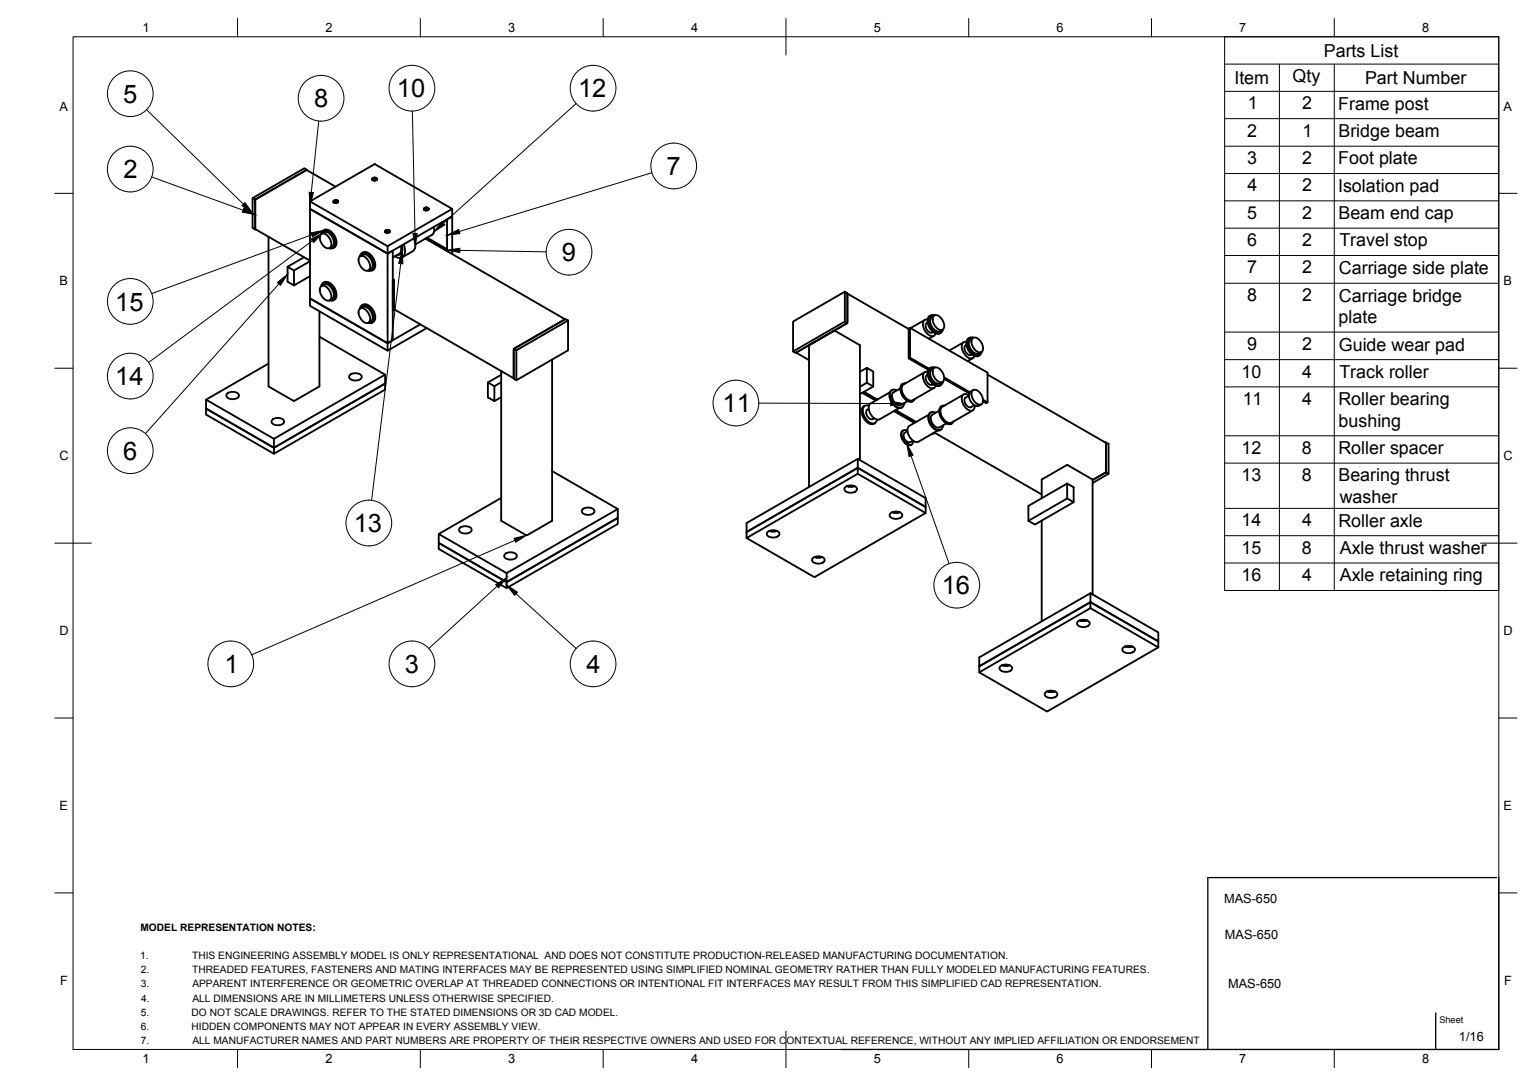
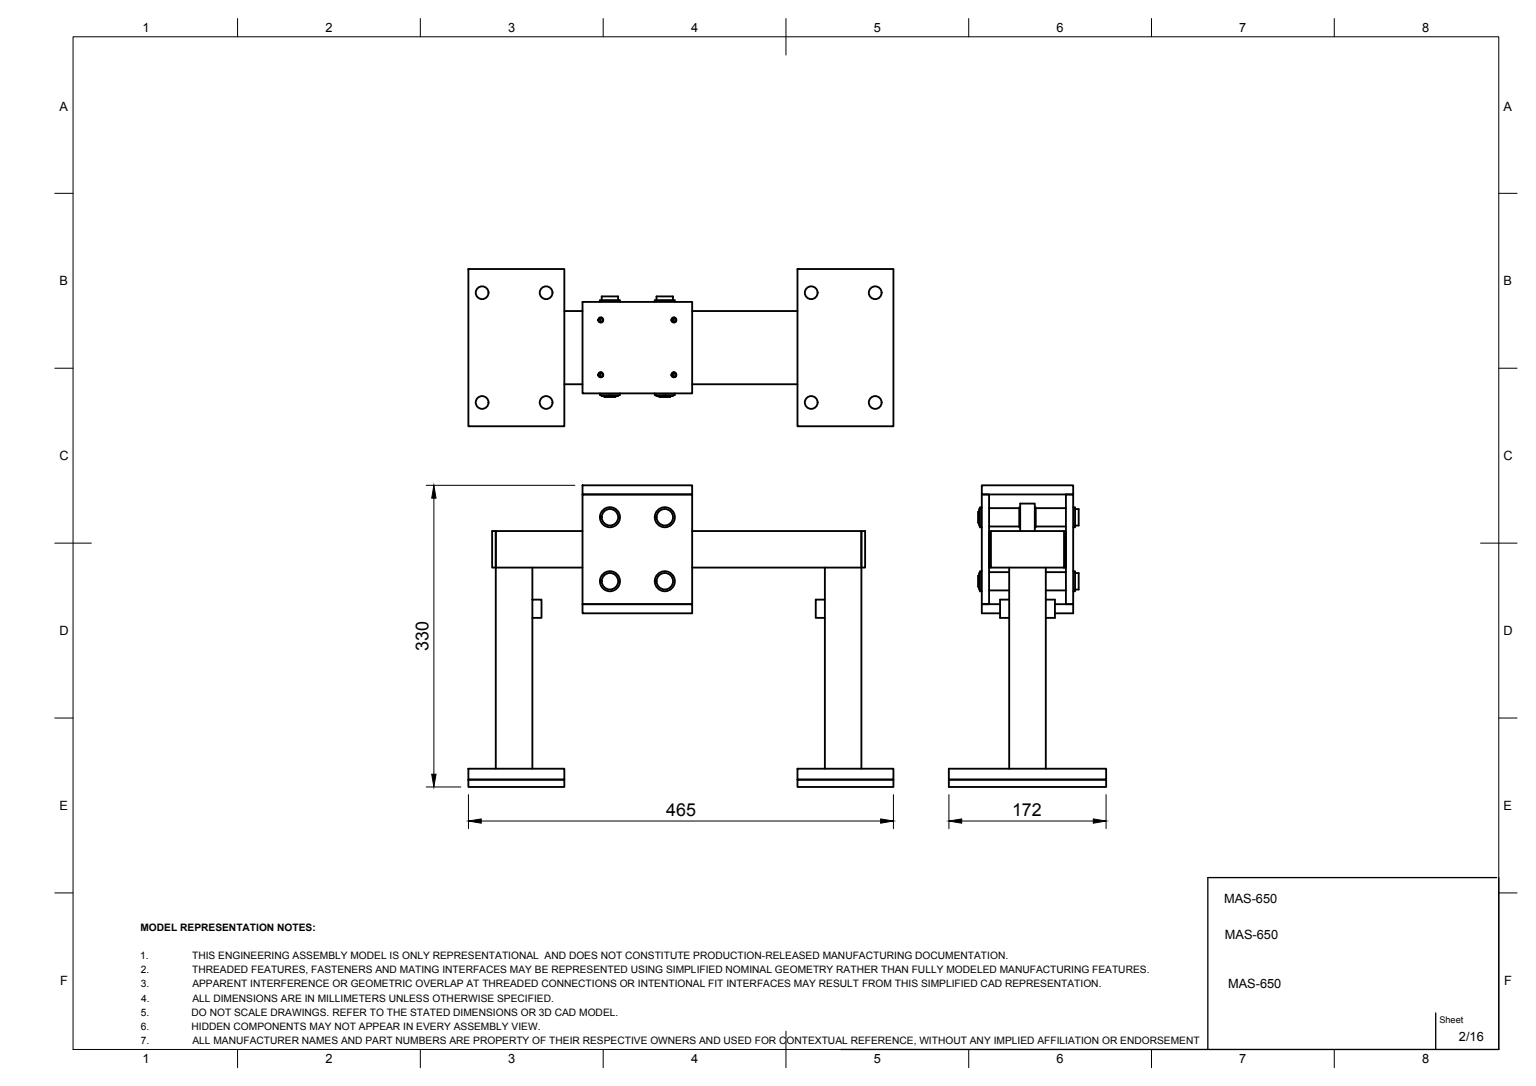
ISO-10303-21;
HEADER;
/* Generated by software containing ST-Developer
 * from STEP Tools, Inc. (www.steptools.com) 
 */

FILE_DESCRIPTION(
/* description */ ('Independent manual traversing gantry with native reusable aluminum pr
ofiles,180mm captured carriage travel, four bronze-bushed rollers, lin
ked ideal rolling motion, bonded acetal lateral guides, positive welde
d end stops and fully retained axle stacks. Editable native profile cu
t lengths220/400mm. Tool attachments viaM6 bridge-plate taps; mounted 
tool outside assembly. Welds, anchors, adhesives, fits, traction, load
/speed/structural/life ratings unassigned.'),
/* implementation_level */ '2;1');

FILE_NAME(
/* name */ 'MAS-650.step',
/* time_stamp */ '2026-11-09T20:04:38-08:00',
/* author */ (''),
/* organization */ (''),
/* preprocessor_version */ 'ST-DEVELOPER v20.2',
/* originating_system */ 'Autodesk Translation Framework v15.17.0.0',
/* authorisation */ '');

FILE_SCHEMA (('AUTOMOTIVE_DESIGN { 1 0 10303 214 3 1 1 }'));
ENDSEC;

DATA;
#10=MECHANICAL_DESIGN_GEOMETRIC_PRESENTATION_REPRESENTATION('',(#471,#472,
#473,#474,#475,#476,#477,#478,#479,#480,#481,#482,#483,#484,#485,#486),
#13231);
#11=ITEM_DEFINED_TRANSFORMATION($,$,#4380,#4678);
#12=ITEM_DEFINED_TRANSFORMATION($,$,#4345,#4679);
#13=ITEM_DEFINED_TRANSFORMATION($,$,#4380,#4680);
#14=ITEM_DEFINED_TRANSFORMATION($,$,#4415,#4681);
#15=ITEM_DEFINED_TRANSFORMATION($,$,#4434,#4682);
#16=ITEM_DEFINED_TRANSFORMATION($,$,#4453,#4683);
#17=ITEM_DEFINED_TRANSFORMATION($,$,#4460,#4684);
#18=ITEM_DEFINED_TRANSFORMATION($,$,#4467,#4685);
#19=ITEM_DEFINED_TRANSFORMATION($,$,#4486,#4686);
#20=ITEM_DEFINED_TRANSFORMATION($,$,#4597,#4687);
#21=ITEM_DEFINED_TRANSFORMATION($,$,#4604,#4688);
#22=ITEM_DEFINED_TRANSFORMATION($,$,#4613,#4689);
#23=ITEM_DEFINED_TRANSFORMATION($,$,#4651,#4690);
#24=ITEM_DEFINED_TRANSFORMATION($,$,#4660,#4691);
#25=ITEM_DEFINED_TRANSFORMATION($,$,#4622,#4692);
#26=ITEM_DEFINED_TRANSFORMATION($,$,#4669,#4693);
#27=ITEM_DEFINED_TRANSFORMATION($,$,#4640,#4694);
#28=ITEM_DEFINED_TRANSFORMATION($,$,#4415,#4695);
#29=ITEM_DEFINED_TRANSFORMATION($,$,#4434,#4696);
#30=ITEM_DEFINED_TRANSFORMATION($,$,#4453,#4697);
#31=ITEM_DEFINED_TRANSFORMATION($,$,#4460,#4698);
#32=ITEM_DEFINED_TRANSFORMATION($,$,#4467,#4699);
#33=ITEM_DEFINED_TRANSFORMATION($,$,#4486,#4700);
#34=ITEM_DEFINED_TRANSFORMATION($,$,#4597,#4701);
#35=ITEM_DEFINED_TRANSFORMATION($,$,#4651,#4702);
#36=ITEM_DEFINED_TRANSFORMATION($,$,#4660,#4703);
#37=ITEM_DEFINED_TRANSFORMATION($,$,#4669,#4704);
#38=ITEM_DEFINED_TRANSFORMATION($,$,#4604,#4705);
#39=ITEM_DEFINED_TRANSFORMATION($,$,#4613,#4706);
#40=ITEM_DEFINED_TRANSFORMATION($,$,#4622,#4707);
#41=ITEM_DEFINED_TRANSFORMATION($,$,#4640,#4708);
#42=ITEM_DEFINED_TRANSFORMATION($,$,#4651,#4709);
#43=ITEM_DEFINED_TRANSFORMATION($,$,#4651,#4710);
#44=ITEM_DEFINED_TRANSFORMATION($,$,#4660,#4711);
#45=ITEM_DEFINED_TRANSFORMATION($,$,#4660,#4712);
#46=ITEM_DEFINED_TRANSFORMATION($,$,#4669,#4713);
#47=ITEM_DEFINED_TRANSFORMATION($,$,#4669,#4714);
#48=ITEM_DEFINED_TRANSFORMATION($,$,#4604,#4715);
#49=ITEM_DEFINED_TRANSFORMATION($,$,#4613,#4716);
#50=ITEM_DEFINED_TRANSFORMATION($,$,#4622,#4717);
#51=ITEM_DEFINED_TRANSFORMATION($,$,#4640,#4718);
#52=ITEM_DEFINED_TRANSFORMATION($,$,#4651,#4719);
#53=ITEM_DEFINED_TRANSFORMATION($,$,#4651,#4720);
#54=ITEM_DEFINED_TRANSFORMATION($,$,#4660,#4721);
#55=ITEM_DEFINED_TRANSFORMATION($,$,#4660,#4722);
#56=ITEM_DEFINED_TRANSFORMATION($,$,#4669,#4723);
#57=ITEM_DEFINED_TRANSFORMATION($,$,#4669,#4724);
#58=ITEM_DEFINED_TRANSFORMATION($,$,#4604,#4725);
#59=ITEM_DEFINED_TRANSFORMATION($,$,#4613,#4726);
#60=ITEM_DEFINED_TRANSFORMATION($,$,#4622,#4727);
#61=ITEM_DEFINED_TRANSFORMATION($,$,#4640,#4728);
#62=ITEM_DEFINED_TRANSFORMATION($,$,#4651,#4729);
#63=ITEM_DEFINED_TRANSFORMATION($,$,#4651,#4730);
#64=ITEM_DEFINED_TRANSFORMATION($,$,#4660,#4731);
#65=ITEM_DEFINED_TRANSFORMATION($,$,#4660,#4732);
#66=ITEM_DEFINED_TRANSFORMATION($,$,#4669,#4733);
#67=ITEM_DEFINED_TRANSFORMATION($,$,#4669,#4734);
#68=(
REPRESENTATION_RELATIONSHIP($,$,#13329,#13327)
REPRESENTATION_RELATIONSHIP_WITH_TRANSFORMATION(#11)
SHAPE_REPRESENTATION_RELATIONSHIP()
);
#69=(
REPRESENTATION_RELATIONSHIP($,$,#13328,#13327)
REPRESENTATION_RELATIONSHIP_WITH_TRANSFORMATION(#12)
SHAPE_REPRESENTATION_RELATIONSHIP()
);
#70=(
REPRESENTATION_RELATIONSHIP($,$,#13329,#13327)
REPRESENTATION_RELATIONSHIP_WITH_TRANSFORMATION(#13)
SHAPE_REPRESENTATION_RELATIONSHIP()
);
#71=(
REPRESENTATION_RELATIONSHIP($,$,#13330,#13327)
REPRESENTATION_RELATIONSHIP_WITH_TRANSFORMATION(#14)
SHAPE_REPRESENTATION_RELATIONSHIP()
);
#72=(
REPRESENTATION_RELATIONSHIP($,$,#13331,#13327)
REPRESENTATION_RELATIONSHIP_WITH_TRANSFORMATION(#15)
SHAPE_REPRESENTATION_RELATIONSHIP()
);
#73=(
REPRESENTATION_RELATIONSHIP($,$,#13332,#13327)
REPRESENTATION_RELATIONSHIP_WITH_TRANSFORMATION(#16)
SHAPE_REPRESENTATION_RELATIONSHIP()
);
#74=(
REPRESENTATION_RELATIONSHIP($,$,#13333,#13327)
REPRESENTATION_RELATIONSHIP_WITH_TRANSFORMATION(#17)
SHAPE_REPRESENTATION_RELATIONSHIP()
);
#75=(
REPRESENTATION_RELATIONSHIP($,$,#13334,#13327)
REPRESENTATION_RELATIONSHIP_WITH_TRANSFORMATION(#18)
SHAPE_REPRESENTATION_RELATIONSHIP()
);
#76=(
REPRESENTATION_RELATIONSHIP($,$,#13335,#13327)
REPRESENTATION_RELATIONSHIP_WITH_TRANSFORMATION(#19)
SHAPE_REPRESENTATION_RELATIONSHIP()
);
#77=(
REPRESENTATION_RELATIONSHIP($,$,#13336,#13327)
REPRESENTATION_RELATIONSHIP_WITH_TRANSFORMATION(#20)
SHAPE_REPRESENTATION_RELATIONSHIP()
);
#78=(
REPRESENTATION_RELATIONSHIP($,$,#13337,#13327)
REPRESENTATION_RELATIONSHIP_WITH_TRANSFORMATION(#21)
SHAPE_REPRESENTATION_RELATIONSHIP()
);
#79=(
REPRESENTATION_RELATIONSHIP($,$,#13338,#13327)
REPRESENTATION_RELATIONSHIP_WITH_TRANSFORMATION(#22)
SHAPE_REPRESENTATION_RELATIONSHIP()
);
#80=(
REPRESENTATION_RELATIONSHIP($,$,#13341,#13327)
REPRESENTATION_RELATIONSHIP_WITH_TRANSFORMATION(#23)
SHAPE_REPRESENTATION_RELATIONSHIP()
);
#81=(
REPRESENTATION_RELATIONSHIP($,$,#13342,#13327)
REPRESENTATION_RELATIONSHIP_WITH_TRANSFORMATION(#24)
SHAPE_REPRESENTATION_RELATIONSHIP()
);
#82=(
REPRESENTATION_RELATIONSHIP($,$,#13339,#13327)
REPRESENTATION_RELATIONSHIP_WITH_TRANSFORMATION(#25)
SHAPE_REPRESENTATION_RELATIONSHIP()
);
#83=(
REPRESENTATION_RELATIONSHIP($,$,#13343,#13327)
REPRESENTATION_RELATIONSHIP_WITH_TRANSFORMATION(#26)
SHAPE_REPRESENTATION_RELATIONSHIP()
);
#84=(
REPRESENTATION_RELATIONSHIP($,$,#13340,#13327)
REPRESENTATION_RELATIONSHIP_WITH_TRANSFORMATION(#27)
SHAPE_REPRESENTATION_RELATIONSHIP()
);
#85=(
REPRESENTATION_RELATIONSHIP($,$,#13330,#13327)
REPRESENTATION_RELATIONSHIP_WITH_TRANSFORMATION(#28)
SHAPE_REPRESENTATION_RELATIONSHIP()
);
#86=(
REPRESENTATION_RELATIONSHIP($,$,#13331,#13327)
REPRESENTATION_RELATIONSHIP_WITH_TRANSFORMATION(#29)
SHAPE_REPRESENTATION_RELATIONSHIP()
);
#87=(
REPRESENTATION_RELATIONSHIP($,$,#13332,#13327)
REPRESENTATION_RELATIONSHIP_WITH_TRANSFORMATION(#30)
SHAPE_REPRESENTATION_RELATIONSHIP()
);
#88=(
REPRESENTATION_RELATIONSHIP($,$,#13333,#13327)
REPRESENTATION_RELATIONSHIP_WITH_TRANSFORMATION(#31)
SHAPE_REPRESENTATION_RELATIONSHIP()
);
#89=(
REPRESENTATION_RELATIONSHIP($,$,#13334,#13327)
REPRESENTATION_RELATIONSHIP_WITH_TRANSFORMATION(#32)
SHAPE_REPRESENTATION_RELATIONSHIP()
);
#90=(
REPRESENTATION_RELATIONSHIP($,$,#13335,#13327)
REPRESENTATION_RELATIONSHIP_WITH_TRANSFORMATION(#33)
SHAPE_REPRESENTATION_RELATIONSHIP()
);
#91=(
REPRESENTATION_RELATIONSHIP($,$,#13336,#13327)
REPRESENTATION_RELATIONSHIP_WITH_TRANSFORMATION(#34)
SHAPE_REPRESENTATION_RELATIONSHIP()
);
#92=(
REPRESENTATION_RELATIONSHIP($,$,#13341,#13327)
REPRESENTATION_RELATIONSHIP_WITH_TRANSFORMATION(#35)
SHAPE_REPRESENTATION_RELATIONSHIP()
);
#93=(
REPRESENTATION_RELATIONSHIP($,$,#13342,#13327)
REPRESENTATION_RELATIONSHIP_WITH_TRANSFORMATION(#36)
SHAPE_REPRESENTATION_RELATIONSHIP()
);
#94=(
REPRESENTATION_RELATIONSHIP($,$,#13343,#13327)
REPRESENTATION_RELATIONSHIP_WITH_TRANSFORMATION(#37)
SHAPE_REPRESENTATION_RELATIONSHIP()
);
#95=(
REPRESENTATION_RELATIONSHIP($,$,#13337,#13327)
REPRESENTATION_RELATIONSHIP_WITH_TRANSFORMATION(#38)
SHAPE_REPRESENTATION_RELATIONSHIP()
);
#96=(
REPRESENTATION_RELATIONSHIP($,$,#13338,#13327)
REPRESENTATION_RELATIONSHIP_WITH_TRANSFORMATION(#39)
SHAPE_REPRESENTATION_RELATIONSHIP()
);
#97=(
REPRESENTATION_RELATIONSHIP($,$,#13339,#13327)
REPRESENTATION_RELATIONSHIP_WITH_TRANSFORMATION(#40)
SHAPE_REPRESENTATION_RELATIONSHIP()
);
#98=(
REPRESENTATION_RELATIONSHIP($,$,#13340,#13327)
REPRESENTATION_RELATIONSHIP_WITH_TRANSFORMATION(#41)
SHAPE_REPRESENTATION_RELATIONSHIP()
);
#99=(
REPRESENTATION_RELATIONSHIP($,$,#13341,#13327)
REPRESENTATION_RELATIONSHIP_WITH_TRANSFORMATION(#42)
SHAPE_REPRESENTATION_RELATIONSHIP()
);
#100=(
REPRESENTATION_RELATIONSHIP($,$,#13341,#13327)
REPRESENTATION_RELATIONSHIP_WITH_TRANSFORMATION(#43)
SHAPE_REPRESENTATION_RELATIONSHIP()
);
#101=(
REPRESENTATION_RELATIONSHIP($,$,#13342,#13327)
REPRESENTATION_RELATIONSHIP_WITH_TRANSFORMATION(#44)
SHAPE_REPRESENTATION_RELATIONSHIP()
);
#102=(
REPRESENTATION_RELATIONSHIP($,$,#13342,#13327)
REPRESENTATION_RELATIONSHIP_WITH_TRANSFORMATION(#45)
SHAPE_REPRESENTATION_RELATIONSHIP()
);
#103=(
REPRESENTATION_RELATIONSHIP($,$,#13343,#13327)
REPRESENTATION_RELATIONSHIP_WITH_TRANSFORMATION(#46)
SHAPE_REPRESENTATION_RELATIONSHIP()
);
#104=(
REPRESENTATION_RELATIONSHIP($,$,#13343,#13327)
REPRESENTATION_RELATIONSHIP_WITH_TRANSFORMATION(#47)
SHAPE_REPRESENTATION_RELATIONSHIP()
);
#105=(
REPRESENTATION_RELATIONSHIP($,$,#13337,#13327)
REPRESENTATION_RELATIONSHIP_WITH_TRANSFORMATION(#48)
SHAPE_REPRESENTATION_RELATIONSHIP()
);
#106=(
REPRESENTATION_RELATIONSHIP($,$,#13338,#13327)
REPRESENTATION_RELATIONSHIP_WITH_TRANSFORMATION(#49)
SHAPE_REPRESENTATION_RELATIONSHIP()
);
#107=(
REPRESENTATION_RELATIONSHIP($,$,#13339,#13327)
REPRESENTATION_RELATIONSHIP_WITH_TRANSFORMATION(#50)
SHAPE_REPRESENTATION_RELATIONSHIP()
);
#108=(
REPRESENTATION_RELATIONSHIP($,$,#13340,#13327)
REPRESENTATION_RELATIONSHIP_WITH_TRANSFORMATION(#51)
SHAPE_REPRESENTATION_RELATIONSHIP()
);
#109=(
REPRESENTATION_RELATIONSHIP($,$,#13341,#13327)
REPRESENTATION_RELATIONSHIP_WITH_TRANSFORMATION(#52)
SHAPE_REPRESENTATION_RELATIONSHIP()
);
#110=(
REPRESENTATION_RELATIONSHIP($,$,#13341,#13327)
REPRESENTATION_RELATIONSHIP_WITH_TRANSFORMATION(#53)
SHAPE_REPRESENTATION_RELATIONSHIP()
);
#111=(
REPRESENTATION_RELATIONSHIP($,$,#13342,#13327)
REPRESENTATION_RELATIONSHIP_WITH_TRANSFORMATION(#54)
SHAPE_REPRESENTATION_RELATIONSHIP()
);
#112=(
REPRESENTATION_RELATIONSHIP($,$,#13342,#13327)
REPRESENTATION_RELATIONSHIP_WITH_TRANSFORMATION(#55)
SHAPE_REPRESENTATION_RELATIONSHIP()
);
#113=(
REPRESENTATION_RELATIONSHIP($,$,#13343,#13327)
REPRESENTATION_RELATIONSHIP_WITH_TRANSFORMATION(#56)
SHAPE_REPRESENTATION_RELATIONSHIP()
);
#114=(
REPRESENTATION_RELATIONSHIP($,$,#13343,#13327)
REPRESENTATION_RELATIONSHIP_WITH_TRANSFORMATION(#57)
SHAPE_REPRESENTATION_RELATIONSHIP()
);
#115=(
REPRESENTATION_RELATIONSHIP($,$,#13337,#13327)
REPRESENTATION_RELATIONSHIP_WITH_TRANSFORMATION(#58)
SHAPE_REPRESENTATION_RELATIONSHIP()
);
#116=(
REPRESENTATION_RELATIONSHIP($,$,#13338,#13327)
REPRESENTATION_RELATIONSHIP_WITH_TRANSFORMATION(#59)
SHAPE_REPRESENTATION_RELATIONSHIP()
);
#117=(
REPRESENTATION_RELATIONSHIP($,$,#13339,#13327)
REPRESENTATION_RELATIONSHIP_WITH_TRANSFORMATION(#60)
SHAPE_REPRESENTATION_RELATIONSHIP()
);
#118=(
REPRESENTATION_RELATIONSHIP($,$,#13340,#13327)
REPRESENTATION_RELATIONSHIP_WITH_TRANSFORMATION(#61)
SHAPE_REPRESENTATION_RELATIONSHIP()
);
#119=(
REPRESENTATION_RELATIONSHIP($,$,#13341,#13327)
REPRESENTATION_RELATIONSHIP_WITH_TRANSFORMATION(#62)
SHAPE_REPRESENTATION_RELATIONSHIP()
);
#120=(
REPRESENTATION_RELATIONSHIP($,$,#13341,#13327)
REPRESENTATION_RELATIONSHIP_WITH_TRANSFORMATION(#63)
SHAPE_REPRESENTATION_RELATIONSHIP()
);
#121=(
REPRESENTATION_RELATIONSHIP($,$,#13342,#13327)
REPRESENTATION_RELATIONSHIP_WITH_TRANSFORMATION(#64)
SHAPE_REPRESENTATION_RELATIONSHIP()
);
#122=(
REPRESENTATION_RELATIONSHIP($,$,#13342,#13327)
REPRESENTATION_RELATIONSHIP_WITH_TRANSFORMATION(#65)
SHAPE_REPRESENTATION_RELATIONSHIP()
);
#123=(
REPRESENTATION_RELATIONSHIP($,$,#13343,#13327)
REPRESENTATION_RELATIONSHIP_WITH_TRANSFORMATION(#66)
SHAPE_REPRESENTATION_RELATIONSHIP()
);
#124=(
REPRESENTATION_RELATIONSHIP($,$,#13343,#13327)
REPRESENTATION_RELATIONSHIP_WITH_TRANSFORMATION(#67)
SHAPE_REPRESENTATION_RELATIONSHIP()
);
#125=CONTEXT_DEPENDENT_SHAPE_REPRESENTATION(#68,#13270);
#126=CONTEXT_DEPENDENT_SHAPE_REPRESENTATION(#69,#13271);
#127=CONTEXT_DEPENDENT_SHAPE_REPRESENTATION(#70,#13272);
#128=CONTEXT_DEPENDENT_SHAPE_REPRESENTATION(#71,#13273);
#129=CONTEXT_DEPENDENT_SHAPE_REPRESENTATION(#72,#13274);
#130=CONTEXT_DEPENDENT_SHAPE_REPRESENTATION(#73,#13275);
#131=CONTEXT_DEPENDENT_SHAPE_REPRESENTATION(#74,#13276);
#132=CONTEXT_DEPENDENT_SHAPE_REPRESENTATION(#75,#13277);
#133=CONTEXT_DEPENDENT_SHAPE_REPRESENTATION(#76,#13278);
#134=CONTEXT_DEPENDENT_SHAPE_REPRESENTATION(#77,#13279);
#135=CONTEXT_DEPENDENT_SHAPE_REPRESENTATION(#78,#13280);
#136=CONTEXT_DEPENDENT_SHAPE_REPRESENTATION(#79,#13281);
#137=CONTEXT_DEPENDENT_SHAPE_REPRESENTATION(#80,#13282);
#138=CONTEXT_DEPENDENT_SHAPE_REPRESENTATION(#81,#13283);
#139=CONTEXT_DEPENDENT_SHAPE_REPRESENTATION(#82,#13284);
#140=CONTEXT_DEPENDENT_SHAPE_REPRESENTATION(#83,#13285);
#141=CONTEXT_DEPENDENT_SHAPE_REPRESENTATION(#84,#13286);
#142=CONTEXT_DEPENDENT_SHAPE_REPRESENTATION(#85,#13287);
#143=CONTEXT_DEPENDENT_SHAPE_REPRESENTATION(#86,#13288);
#144=CONTEXT_DEPENDENT_SHAPE_REPRESENTATION(#87,#13289);
#145=CONTEXT_DEPENDENT_SHAPE_REPRESENTATION(#88,#13290);
#146=CONTEXT_DEPENDENT_SHAPE_REPRESENTATION(#89,#13291);
#147=CONTEXT_DEPENDENT_SHAPE_REPRESENTATION(#90,#13292);
#148=CONTEXT_DEPENDENT_SHAPE_REPRESENTATION(#91,#13293);
#149=CONTEXT_DEPENDENT_SHAPE_REPRESENTATION(#92,#13294);
#150=CONTEXT_DEPENDENT_SHAPE_REPRESENTATION(#93,#13295);
#151=CONTEXT_DEPENDENT_SHAPE_REPRESENTATION(#94,#13296);
#152=CONTEXT_DEPENDENT_SHAPE_REPRESENTATION(#95,#13297);
#153=CONTEXT_DEPENDENT_SHAPE_REPRESENTATION(#96,#13298);
#154=CONTEXT_DEPENDENT_SHAPE_REPRESENTATION(#97,#13299);
#155=CONTEXT_DEPENDENT_SHAPE_REPRESENTATION(#98,#13300);
#156=CONTEXT_DEPENDENT_SHAPE_REPRESENTATION(#99,#13301);
#157=CONTEXT_DEPENDENT_SHAPE_REPRESENTATION(#100,#13302);
#158=CONTEXT_DEPENDENT_SHAPE_REPRESENTATION(#101,#13303);
#159=CONTEXT_DEPENDENT_SHAPE_REPRESENTATION(#102,#13304);
#160=CONTEXT_DEPENDENT_SHAPE_REPRESENTATION(#103,#13305);
#161=CONTEXT_DEPENDENT_SHAPE_REPRESENTATION(#104,#13306);
#162=CONTEXT_DEPENDENT_SHAPE_REPRESENTATION(#105,#13307);
#163=CONTEXT_DEPENDENT_SHAPE_REPRESENTATION(#106,#13308);
#164=CONTEXT_DEPENDENT_SHAPE_REPRESENTATION(#107,#13309);
#165=CONTEXT_DEPENDENT_SHAPE_REPRESENTATION(#108,#13310);
#166=CONTEXT_DEPENDENT_SHAPE_REPRESENTATION(#109,#13311);
#167=CONTEXT_DEPENDENT_SHAPE_REPRESENTATION(#110,#13312);
#168=CONTEXT_DEPENDENT_SHAPE_REPRESENTATION(#111,#13313);
#169=CONTEXT_DEPENDENT_SHAPE_REPRESENTATION(#112,#13314);
#170=CONTEXT_DEPENDENT_SHAPE_REPRESENTATION(#113,#13315);
#171=CONTEXT_DEPENDENT_SHAPE_REPRESENTATION(#114,#13316);
#172=CONTEXT_DEPENDENT_SHAPE_REPRESENTATION(#115,#13317);
#173=CONTEXT_DEPENDENT_SHAPE_REPRESENTATION(#116,#13318);
#174=CONTEXT_DEPENDENT_SHAPE_REPRESENTATION(#117,#13319);
#175=CONTEXT_DEPENDENT_SHAPE_REPRESENTATION(#118,#13320);
#176=CONTEXT_DEPENDENT_SHAPE_REPRESENTATION(#119,#13321);
#177=CONTEXT_DEPENDENT_SHAPE_REPRESENTATION(#120,#13322);
#178=CONTEXT_DEPENDENT_SHAPE_REPRESENTATION(#121,#13323);
#179=CONTEXT_DEPENDENT_SHAPE_REPRESENTATION(#122,#13324);
#180=CONTEXT_DEPENDENT_SHAPE_REPRESENTATION(#123,#13325);
#181=CONTEXT_DEPENDENT_SHAPE_REPRESENTATION(#124,#13326);
#182=NEXT_ASSEMBLY_USAGE_OCCURRENCE('Frame post:1','Frame post:1',
'Frame post:1',#13345,#13347,'Frame post:1');
#183=NEXT_ASSEMBLY_USAGE_OCCURRENCE('Bridge beam:1','Bridge beam:1',
'Bridge beam:1',#13345,#13346,'Bridge beam:1');
#184=NEXT_ASSEMBLY_USAGE_OCCURRENCE('Frame post:2','Frame post:2',
'Frame post:2',#13345,#13347,'Frame post:2');
#185=NEXT_ASSEMBLY_USAGE_OCCURRENCE('Foot plate:1','Foot plate:1',
'Foot plate:1',#13345,#13348,'Foot plate:1');
#186=NEXT_ASSEMBLY_USAGE_OCCURRENCE('Isolation pad:1','Isolation pad:1',
'Isolation pad:1',#13345,#13349,'Isolation pad:1');
#187=NEXT_ASSEMBLY_USAGE_OCCURRENCE('Beam end cap:1','Beam end cap:1',
'Beam end cap:1',#13345,#13350,'Beam end cap:1');
#188=NEXT_ASSEMBLY_USAGE_OCCURRENCE('Travel stop:1','Travel stop:1',
'Travel stop:1',#13345,#13351,'Travel stop:1');
#189=NEXT_ASSEMBLY_USAGE_OCCURRENCE('Carriage side plate:1',
'Carriage side plate:1','Carriage side plate:1',#13345,#13352,
'Carriage side plate:1');
#190=NEXT_ASSEMBLY_USAGE_OCCURRENCE('Carriage bridge plate:1',
'Carriage bridge plate:1','Carriage bridge plate:1',#13345,#13353,
'Carriage bridge plate:1');
#191=NEXT_ASSEMBLY_USAGE_OCCURRENCE('Guide wear pad:1',
'Guide wear pad:1','Guide wear pad:1',#13345,#13354,'Guide wear pad:1');
#192=NEXT_ASSEMBLY_USAGE_OCCURRENCE('Track roller:1','Track roller:1',
'Track roller:1',#13345,#13355,'Track roller:1');
#193=NEXT_ASSEMBLY_USAGE_OCCURRENCE('Roller bearing bushing:1',
'Roller bearing bushing:1','Roller bearing bushing:1',#13345,#13356,
'Roller bearing bushing:1');
#194=NEXT_ASSEMBLY_USAGE_OCCURRENCE('Roller spacer:1','Roller spacer:1',
'Roller spacer:1',#13345,#13359,'Roller spacer:1');
#195=NEXT_ASSEMBLY_USAGE_OCCURRENCE('Bearing thrust washer:1',
'Bearing thrust washer:1','Bearing thrust washer:1',#13345,#13360,
'Bearing thrust washer:1');
#196=NEXT_ASSEMBLY_USAGE_OCCURRENCE('Roller axle:1','Roller axle:1',
'Roller axle:1',#13345,#13357,'Roller axle:1');
#197=NEXT_ASSEMBLY_USAGE_OCCURRENCE('Axle thrust washer:1',
'Axle thrust washer:1','Axle thrust washer:1',#13345,#13361,
'Axle thrust washer:1');
#198=NEXT_ASSEMBLY_USAGE_OCCURRENCE('Axle retaining ring:1',
'Axle retaining ring:1','Axle retaining ring:1',#13345,#13358,
'Axle retaining ring:1');
#199=NEXT_ASSEMBLY_USAGE_OCCURRENCE('Foot plate:2','Foot plate:2',
'Foot plate:2',#13345,#13348,'Foot plate:2');
#200=NEXT_ASSEMBLY_USAGE_OCCURRENCE('Isolation pad:2','Isolation pad:2',
'Isolation pad:2',#13345,#13349,'Isolation pad:2');
#201=NEXT_ASSEMBLY_USAGE_OCCURRENCE('Beam end cap:2','Beam end cap:2',
'Beam end cap:2',#13345,#13350,'Beam end cap:2');
#202=NEXT_ASSEMBLY_USAGE_OCCURRENCE('Travel stop:2','Travel stop:2',
'Travel stop:2',#13345,#13351,'Travel stop:2');
#203=NEXT_ASSEMBLY_USAGE_OCCURRENCE('Carriage side plate:2',
'Carriage side plate:2','Carriage side plate:2',#13345,#13352,
'Carriage side plate:2');
#204=NEXT_ASSEMBLY_USAGE_OCCURRENCE('Carriage bridge plate:2',
'Carriage bridge plate:2','Carriage bridge plate:2',#13345,#13353,
'Carriage bridge plate:2');
#205=NEXT_ASSEMBLY_USAGE_OCCURRENCE('Guide wear pad:2',
'Guide wear pad:2','Guide wear pad:2',#13345,#13354,'Guide wear pad:2');
#206=NEXT_ASSEMBLY_USAGE_OCCURRENCE('Roller spacer:2','Roller spacer:2',
'Roller spacer:2',#13345,#13359,'Roller spacer:2');
#207=NEXT_ASSEMBLY_USAGE_OCCURRENCE('Bearing thrust washer:2',
'Bearing thrust washer:2','Bearing thrust washer:2',#13345,#13360,
'Bearing thrust washer:2');
#208=NEXT_ASSEMBLY_USAGE_OCCURRENCE('Axle thrust washer:2',
'Axle thrust washer:2','Axle thrust washer:2',#13345,#13361,
'Axle thrust washer:2');
#209=NEXT_ASSEMBLY_USAGE_OCCURRENCE('Track roller:2','Track roller:2',
'Track roller:2',#13345,#13355,'Track roller:2');
#210=NEXT_ASSEMBLY_USAGE_OCCURRENCE('Roller bearing bushing:2',
'Roller bearing bushing:2','Roller bearing bushing:2',#13345,#13356,
'Roller bearing bushing:2');
#211=NEXT_ASSEMBLY_USAGE_OCCURRENCE('Roller axle:2','Roller axle:2',
'Roller axle:2',#13345,#13357,'Roller axle:2');
#212=NEXT_ASSEMBLY_USAGE_OCCURRENCE('Axle retaining ring:2',
'Axle retaining ring:2','Axle retaining ring:2',#13345,#13358,
'Axle retaining ring:2');
#213=NEXT_ASSEMBLY_USAGE_OCCURRENCE('Roller spacer:3','Roller spacer:3',
'Roller spacer:3',#13345,#13359,'Roller spacer:3');
#214=NEXT_ASSEMBLY_USAGE_OCCURRENCE('Roller spacer:4','Roller spacer:4',
'Roller spacer:4',#13345,#13359,'Roller spacer:4');
#215=NEXT_ASSEMBLY_USAGE_OCCURRENCE('Bearing thrust washer:3',
'Bearing thrust washer:3','Bearing thrust washer:3',#13345,#13360,
'Bearing thrust washer:3');
#216=NEXT_ASSEMBLY_USAGE_OCCURRENCE('Bearing thrust washer:4',
'Bearing thrust washer:4','Bearing thrust washer:4',#13345,#13360,
'Bearing thrust washer:4');
#217=NEXT_ASSEMBLY_USAGE_OCCURRENCE('Axle thrust washer:3',
'Axle thrust washer:3','Axle thrust washer:3',#13345,#13361,
'Axle thrust washer:3');
#218=NEXT_ASSEMBLY_USAGE_OCCURRENCE('Axle thrust washer:4',
'Axle thrust washer:4','Axle thrust washer:4',#13345,#13361,
'Axle thrust washer:4');
#219=NEXT_ASSEMBLY_USAGE_OCCURRENCE('Track roller:3','Track roller:3',
'Track roller:3',#13345,#13355,'Track roller:3');
#220=NEXT_ASSEMBLY_USAGE_OCCURRENCE('Roller bearing bushing:3',
'Roller bearing bushing:3','Roller bearing bushing:3',#13345,#13356,
'Roller bearing bushing:3');
#221=NEXT_ASSEMBLY_USAGE_OCCURRENCE('Roller axle:3','Roller axle:3',
'Roller axle:3',#13345,#13357,'Roller axle:3');
#222=NEXT_ASSEMBLY_USAGE_OCCURRENCE('Axle retaining ring:3',
'Axle retaining ring:3','Axle retaining ring:3',#13345,#13358,
'Axle retaining ring:3');
#223=NEXT_ASSEMBLY_USAGE_OCCURRENCE('Roller spacer:5','Roller spacer:5',
'Roller spacer:5',#13345,#13359,'Roller spacer:5');
#224=NEXT_ASSEMBLY_USAGE_OCCURRENCE('Roller spacer:6','Roller spacer:6',
'Roller spacer:6',#13345,#13359,'Roller spacer:6');
#225=NEXT_ASSEMBLY_USAGE_OCCURRENCE('Bearing thrust washer:5',
'Bearing thrust washer:5','Bearing thrust washer:5',#13345,#13360,
'Bearing thrust washer:5');
#226=NEXT_ASSEMBLY_USAGE_OCCURRENCE('Bearing thrust washer:6',
'Bearing thrust washer:6','Bearing thrust washer:6',#13345,#13360,
'Bearing thrust washer:6');
#227=NEXT_ASSEMBLY_USAGE_OCCURRENCE('Axle thrust washer:5',
'Axle thrust washer:5','Axle thrust washer:5',#13345,#13361,
'Axle thrust washer:5');
#228=NEXT_ASSEMBLY_USAGE_OCCURRENCE('Axle thrust washer:6',
'Axle thrust washer:6','Axle thrust washer:6',#13345,#13361,
'Axle thrust washer:6');
#229=NEXT_ASSEMBLY_USAGE_OCCURRENCE('Track roller:4','Track roller:4',
'Track roller:4',#13345,#13355,'Track roller:4');
#230=NEXT_ASSEMBLY_USAGE_OCCURRENCE('Roller bearing bushing:4',
'Roller bearing bushing:4','Roller bearing bushing:4',#13345,#13356,
'Roller bearing bushing:4');
#231=NEXT_ASSEMBLY_USAGE_OCCURRENCE('Roller axle:4','Roller axle:4',
'Roller axle:4',#13345,#13357,'Roller axle:4');
#232=NEXT_ASSEMBLY_USAGE_OCCURRENCE('Axle retaining ring:4',
'Axle retaining ring:4','Axle retaining ring:4',#13345,#13358,
'Axle retaining ring:4');
#233=NEXT_ASSEMBLY_USAGE_OCCURRENCE('Roller spacer:7','Roller spacer:7',
'Roller spacer:7',#13345,#13359,'Roller spacer:7');
#234=NEXT_ASSEMBLY_USAGE_OCCURRENCE('Roller spacer:8','Roller spacer:8',
'Roller spacer:8',#13345,#13359,'Roller spacer:8');
#235=NEXT_ASSEMBLY_USAGE_OCCURRENCE('Bearing thrust washer:7',
'Bearing thrust washer:7','Bearing thrust washer:7',#13345,#13360,
'Bearing thrust washer:7');
#236=NEXT_ASSEMBLY_USAGE_OCCURRENCE('Bearing thrust washer:8',
'Bearing thrust washer:8','Bearing thrust washer:8',#13345,#13360,
'Bearing thrust washer:8');
#237=NEXT_ASSEMBLY_USAGE_OCCURRENCE('Axle thrust washer:7',
'Axle thrust washer:7','Axle thrust washer:7',#13345,#13361,
'Axle thrust washer:7');
#238=NEXT_ASSEMBLY_USAGE_OCCURRENCE('Axle thrust washer:8',
'Axle thrust washer:8','Axle thrust washer:8',#13345,#13361,
'Axle thrust washer:8');
#239=B_SPLINE_SURFACE_WITH_KNOTS('',3,3,((#8992,#8993,#8994,#8995,#8996,
#8997,#8998,#8999,#9000,#9001,#9002,#9003,#9004,#9005,#9006,#9007,#9008,
#9009,#9010,#9011,#9012,#9013,#9014,#9015,#9016,#9017,#9018,#9019,#9020,
#9021,#9022,#9023,#9024,#9025,#9026,#9027,#9028,#9029,#9030,#9031,#9032,
#9033,#9034,#9035,#9036,#9037,#9038,#9039,#9040,#9041,#9042,#9043,#9044,
#9045,#9046,#9047,#9048,#9049,#9050,#9051,#9052,#9053,#9054,#9055,#9056,
#9057,#9058,#9059),(#9060,#9061,#9062,#9063,#9064,#9065,#9066,#9067,#9068,
#9069,#9070,#9071,#9072,#9073,#9074,#9075,#9076,#9077,#9078,#9079,#9080,
#9081,#9082,#9083,#9084,#9085,#9086,#9087,#9088,#9089,#9090,#9091,#9092,
#9093,#9094,#9095,#9096,#9097,#9098,#9099,#9100,#9101,#9102,#9103,#9104,
#9105,#9106,#9107,#9108,#9109,#9110,#9111,#9112,#9113,#9114,#9115,#9116,
#9117,#9118,#9119,#9120,#9121,#9122,#9123,#9124,#9125,#9126,#9127),(#9128,
#9129,#9130,#9131,#9132,#9133,#9134,#9135,#9136,#9137,#9138,#9139,#9140,
#9141,#9142,#9143,#9144,#9145,#9146,#9147,#9148,#9149,#9150,#9151,#9152,
#9153,#9154,#9155,#9156,#9157,#9158,#9159,#9160,#9161,#9162,#9163,#9164,
#9165,#9166,#9167,#9168,#9169,#9170,#9171,#9172,#9173,#9174,#9175,#9176,
#9177,#9178,#9179,#9180,#9181,#9182,#9183,#9184,#9185,#9186,#9187,#9188,
#9189,#9190,#9191,#9192,#9193,#9194,#9195),(#9196,#9197,#9198,#9199,#9200,
#9201,#9202,#9203,#9204,#9205,#9206,#9207,#9208,#9209,#9210,#9211,#9212,
#9213,#9214,#9215,#9216,#9217,#9218,#9219,#9220,#9221,#9222,#9223,#9224,
#9225,#9226,#9227,#9228,#9229,#9230,#9231,#9232,#9233,#9234,#9235,#9236,
#9237,#9238,#9239,#9240,#9241,#9242,#9243,#9244,#9245,#9246,#9247,#9248,
#9249,#9250,#9251,#9252,#9253,#9254,#9255,#9256,#9257,#9258,#9259,#9260,
#9261,#9262,#9263)),.UNSPECIFIED.,.F.,.F.,.F.,(4,4),(4,1,1,1,1,1,1,1,1,
1,1,1,1,1,1,1,1,1,1,1,1,1,1,1,1,1,1,1,1,1,1,1,1,1,1,1,1,1,1,1,1,1,1,1,1,
1,1,1,1,1,1,1,1,1,1,1,1,1,1,1,1,1,1,1,1,4),(0.,0.0642013499338865),(11.8589888623078,
12.8566626771512,13.8543364919947,14.8520103068381,15.8496841216816,16.8473579365251,
17.8450317513685,18.842705566212,19.8403793810554,20.8380531958989,21.8357270107423,
22.8334008255858,23.8310746404292,24.8287484552727,25.8264222701161,26.8240960849596,
27.821769899803,28.8194437146465,29.8171175294899,30.8147913443334,31.8124651591768,
32.8101389740203,33.8078127888637,34.8054866037072,35.8031604185506,36.8008342333941,
37.7985080482375,38.796181863081,39.7938556779244,40.7915294927679,41.7892033076113,
42.7868771224548,43.7845509372982,44.7822247521417,45.7798985669851,46.7775723818286,
47.775246196672,48.7729200115155,49.7705938263589,50.7682676412024,51.7659414560458,
52.7636152708893,53.7612890857327,54.7589629005762,55.7566367154196,56.7543105302631,
57.7519843451065,58.74965815995,59.7473319747934,60.7450057896369,61.7426796044803,
62.7403534193238,63.7380272341672,64.7357010490107,65.7333748638542,66.7310486786976,
67.728722493541,68.7263963083845,69.7240701232279,70.7217439380714,71.7194177529149,
72.7170915677583,73.7147653826018,74.7124391974452,75.7101130122887,76.7077868271321),
 .UNSPECIFIED.);
#240=B_SPLINE_SURFACE_WITH_KNOTS('',3,3,((#9480,#9481,#9482,#9483,#9484,
#9485,#9486,#9487,#9488,#9489,#9490,#9491,#9492,#9493,#9494,#9495,#9496,
#9497,#9498,#9499,#9500,#9501,#9502,#9503,#9504,#9505,#9506,#9507,#9508,
#9509,#9510,#9511,#9512,#9513,#9514,#9515,#9516,#9517,#9518,#9519,#9520,
#9521,#9522,#9523,#9524,#9525,#9526,#9527,#9528,#9529,#9530,#9531,#9532,
#9533,#9534,#9535,#9536,#9537,#9538,#9539,#9540,#9541,#9542,#9543,#9544,
#9545,#9546,#9547),(#9548,#9549,#9550,#9551,#9552,#9553,#9554,#9555,#9556,
#9557,#9558,#9559,#9560,#9561,#9562,#9563,#9564,#9565,#9566,#9567,#9568,
#9569,#9570,#9571,#9572,#9573,#9574,#9575,#9576,#9577,#9578,#9579,#9580,
#9581,#9582,#9583,#9584,#9585,#9586,#9587,#9588,#9589,#9590,#9591,#9592,
#9593,#9594,#9595,#9596,#9597,#9598,#9599,#9600,#9601,#9602,#9603,#9604,
#9605,#9606,#9607,#9608,#9609,#9610,#9611,#9612,#9613,#9614,#9615),(#9616,
#9617,#9618,#9619,#9620,#9621,#9622,#9623,#9624,#9625,#9626,#9627,#9628,
#9629,#9630,#9631,#9632,#9633,#9634,#9635,#9636,#9637,#9638,#9639,#9640,
#9641,#9642,#9643,#9644,#9645,#9646,#9647,#9648,#9649,#9650,#9651,#9652,
#9653,#9654,#9655,#9656,#9657,#9658,#9659,#9660,#9661,#9662,#9663,#9664,
#9665,#9666,#9667,#9668,#9669,#9670,#9671,#9672,#9673,#9674,#9675,#9676,
#9677,#9678,#9679,#9680,#9681,#9682,#9683),(#9684,#9685,#9686,#9687,#9688,
#9689,#9690,#9691,#9692,#9693,#9694,#9695,#9696,#9697,#9698,#9699,#9700,
#9701,#9702,#9703,#9704,#9705,#9706,#9707,#9708,#9709,#9710,#9711,#9712,
#9713,#9714,#9715,#9716,#9717,#9718,#9719,#9720,#9721,#9722,#9723,#9724,
#9725,#9726,#9727,#9728,#9729,#9730,#9731,#9732,#9733,#9734,#9735,#9736,
#9737,#9738,#9739,#9740,#9741,#9742,#9743,#9744,#9745,#9746,#9747,#9748,
#9749,#9750,#9751)),.UNSPECIFIED.,.F.,.F.,.F.,(4,4),(4,1,1,1,1,1,1,1,1,
1,1,1,1,1,1,1,1,1,1,1,1,1,1,1,1,1,1,1,1,1,1,1,1,1,1,1,1,1,1,1,1,1,1,1,1,
1,1,1,1,1,1,1,1,1,1,1,1,1,1,1,1,1,1,1,1,4),(0.,0.0642013499338865),(14.3984001269718,
15.3960739418153,16.3937477566587,17.3914215715022,18.3890953863456,19.3867692011891,
20.3844430160325,21.382116830876,22.3797906457194,23.3774644605629,24.3751382754063,
25.3728120902498,26.3704859050932,27.3681597199367,28.3658335347801,29.3635073496236,
30.361181164467,31.3588549793105,32.3565287941539,33.3542026089974,34.3518764238408,
35.3495502386843,36.3472240535278,37.3448978683712,38.3425716832147,39.3402454980581,
40.3379193129016,41.335593127745,42.3332669425885,43.3309407574319,44.3286145722754,
45.3262883871188,46.3239622019623,47.3216360168057,48.3193098316492,49.3169836464926,
50.3146574613361,51.3123312761795,52.310005091023,53.3076789058664,54.3053527207099,
55.3030265355533,56.3007003503968,57.2983741652402,58.2960479800837,59.2937217949271,
60.2913956097706,61.289069424614,62.2867432394575,63.2844170543009,64.2820908691444,
65.2797646839878,66.2774384988313,67.2751123136747,68.2727861285182,69.2704599433616,
70.2681337582051,71.2658075730485,72.263481387892,73.2611552027354,74.2588290175789,
75.2565028324223,76.2541766472658,77.2518504621092,78.2495242769527,79.2471980917962),
 .UNSPECIFIED.);
#241=B_SPLINE_SURFACE_WITH_KNOTS('',3,3,((#10569,#10570,#10571,#10572,#10573,
#10574,#10575,#10576,#10577,#10578,#10579,#10580,#10581,#10582,#10583,#10584,
#10585,#10586,#10587,#10588,#10589,#10590,#10591,#10592,#10593,#10594,#10595,
#10596,#10597,#10598,#10599,#10600,#10601,#10602,#10603,#10604,#10605,#10606,
#10607,#10608,#10609,#10610,#10611,#10612,#10613,#10614,#10615,#10616,#10617,
#10618,#10619,#10620,#10621,#10622,#10623,#10624,#10625,#10626,#10627,#10628,
#10629,#10630,#10631,#10632,#10633,#10634,#10635,#10636),(#10637,#10638,
#10639,#10640,#10641,#10642,#10643,#10644,#10645,#10646,#10647,#10648,#10649,
#10650,#10651,#10652,#10653,#10654,#10655,#10656,#10657,#10658,#10659,#10660,
#10661,#10662,#10663,#10664,#10665,#10666,#10667,#10668,#10669,#10670,#10671,
#10672,#10673,#10674,#10675,#10676,#10677,#10678,#10679,#10680,#10681,#10682,
#10683,#10684,#10685,#10686,#10687,#10688,#10689,#10690,#10691,#10692,#10693,
#10694,#10695,#10696,#10697,#10698,#10699,#10700,#10701,#10702,#10703,#10704),
(#10705,#10706,#10707,#10708,#10709,#10710,#10711,#10712,#10713,#10714,
#10715,#10716,#10717,#10718,#10719,#10720,#10721,#10722,#10723,#10724,#10725,
#10726,#10727,#10728,#10729,#10730,#10731,#10732,#10733,#10734,#10735,#10736,
#10737,#10738,#10739,#10740,#10741,#10742,#10743,#10744,#10745,#10746,#10747,
#10748,#10749,#10750,#10751,#10752,#10753,#10754,#10755,#10756,#10757,#10758,
#10759,#10760,#10761,#10762,#10763,#10764,#10765,#10766,#10767,#10768,#10769,
#10770,#10771,#10772),(#10773,#10774,#10775,#10776,#10777,#10778,#10779,
#10780,#10781,#10782,#10783,#10784,#10785,#10786,#10787,#10788,#10789,#10790,
#10791,#10792,#10793,#10794,#10795,#10796,#10797,#10798,#10799,#10800,#10801,
#10802,#10803,#10804,#10805,#10806,#10807,#10808,#10809,#10810,#10811,#10812,
#10813,#10814,#10815,#10816,#10817,#10818,#10819,#10820,#10821,#10822,#10823,
#10824,#10825,#10826,#10827,#10828,#10829,#10830,#10831,#10832,#10833,#10834,
#10835,#10836,#10837,#10838,#10839,#10840)),.UNSPECIFIED.,.F.,.F.,.F.,(4,
4),(4,1,1,1,1,1,1,1,1,1,1,1,1,1,1,1,1,1,1,1,1,1,1,1,1,1,1,1,1,1,1,1,1,1,
1,1,1,1,1,1,1,1,1,1,1,1,1,1,1,1,1,1,1,1,1,1,1,1,1,1,1,1,1,1,1,4),(0.,0.0642013499338865),
(11.8589888623078,12.8566626771512,13.8543364919947,14.8520103068381,15.8496841216816,
16.847357936525,17.8450317513685,18.8427055662119,19.8403793810554,20.8380531958989,
21.8357270107423,22.8334008255858,23.8310746404292,24.8287484552727,25.8264222701161,
26.8240960849596,27.821769899803,28.8194437146465,29.8171175294899,30.8147913443334,
31.8124651591768,32.8101389740203,33.8078127888637,34.8054866037072,35.8031604185506,
36.8008342333941,37.7985080482375,38.796181863081,39.7938556779244,40.7915294927679,
41.7892033076113,42.7868771224548,43.7845509372982,44.7822247521417,45.7798985669851,
46.7775723818286,47.775246196672,48.7729200115155,49.7705938263589,50.7682676412024,
51.7659414560458,52.7636152708893,53.7612890857327,54.7589629005762,55.7566367154196,
56.7543105302631,57.7519843451065,58.74965815995,59.7473319747934,60.7450057896369,
61.7426796044803,62.7403534193238,63.7380272341672,64.7357010490107,65.7333748638542,
66.7310486786976,67.728722493541,68.7263963083845,69.7240701232279,70.7217439380714,
71.7194177529149,72.7170915677583,73.7147653826018,74.7124391974452,75.7101130122887,
76.7077868271321),.UNSPECIFIED.);
#242=B_SPLINE_SURFACE_WITH_KNOTS('',3,3,((#10960,#10961,#10962,#10963,#10964,
#10965,#10966,#10967,#10968,#10969,#10970,#10971,#10972,#10973,#10974,#10975,
#10976,#10977,#10978,#10979,#10980,#10981,#10982,#10983,#10984,#10985,#10986,
#10987,#10988,#10989,#10990,#10991,#10992,#10993,#10994,#10995,#10996,#10997,
#10998,#10999,#11000,#11001,#11002,#11003,#11004,#11005,#11006,#11007,#11008,
#11009,#11010,#11011,#11012,#11013,#11014,#11015,#11016,#11017,#11018,#11019,
#11020,#11021,#11022,#11023,#11024,#11025,#11026,#11027),(#11028,#11029,
#11030,#11031,#11032,#11033,#11034,#11035,#11036,#11037,#11038,#11039,#11040,
#11041,#11042,#11043,#11044,#11045,#11046,#11047,#11048,#11049,#11050,#11051,
#11052,#11053,#11054,#11055,#11056,#11057,#11058,#11059,#11060,#11061,#11062,
#11063,#11064,#11065,#11066,#11067,#11068,#11069,#11070,#11071,#11072,#11073,
#11074,#11075,#11076,#11077,#11078,#11079,#11080,#11081,#11082,#11083,#11084,
#11085,#11086,#11087,#11088,#11089,#11090,#11091,#11092,#11093,#11094,#11095),
(#11096,#11097,#11098,#11099,#11100,#11101,#11102,#11103,#11104,#11105,
#11106,#11107,#11108,#11109,#11110,#11111,#11112,#11113,#11114,#11115,#11116,
#11117,#11118,#11119,#11120,#11121,#11122,#11123,#11124,#11125,#11126,#11127,
#11128,#11129,#11130,#11131,#11132,#11133,#11134,#11135,#11136,#11137,#11138,
#11139,#11140,#11141,#11142,#11143,#11144,#11145,#11146,#11147,#11148,#11149,
#11150,#11151,#11152,#11153,#11154,#11155,#11156,#11157,#11158,#11159,#11160,
#11161,#11162,#11163),(#11164,#11165,#11166,#11167,#11168,#11169,#11170,
#11171,#11172,#11173,#11174,#11175,#11176,#11177,#11178,#11179,#11180,#11181,
#11182,#11183,#11184,#11185,#11186,#11187,#11188,#11189,#11190,#11191,#11192,
#11193,#11194,#11195,#11196,#11197,#11198,#11199,#11200,#11201,#11202,#11203,
#11204,#11205,#11206,#11207,#11208,#11209,#11210,#11211,#11212,#11213,#11214,
#11215,#11216,#11217,#11218,#11219,#11220,#11221,#11222,#11223,#11224,#11225,
#11226,#11227,#11228,#11229,#11230,#11231)),.UNSPECIFIED.,.F.,.F.,.F.,(4,
4),(4,1,1,1,1,1,1,1,1,1,1,1,1,1,1,1,1,1,1,1,1,1,1,1,1,1,1,1,1,1,1,1,1,1,
1,1,1,1,1,1,1,1,1,1,1,1,1,1,1,1,1,1,1,1,1,1,1,1,1,1,1,1,1,1,1,4),(0.,0.0642013499338865),
(14.3984001269718,15.3960739418153,16.3937477566587,17.3914215715022,18.3890953863456,
19.3867692011891,20.3844430160325,21.382116830876,22.3797906457194,23.3774644605629,
24.3751382754063,25.3728120902498,26.3704859050932,27.3681597199367,28.3658335347801,
29.3635073496236,30.361181164467,31.3588549793105,32.3565287941539,33.3542026089974,
34.3518764238408,35.3495502386843,36.3472240535278,37.3448978683712,38.3425716832147,
39.3402454980581,40.3379193129016,41.335593127745,42.3332669425885,43.3309407574319,
44.3286145722754,45.3262883871188,46.3239622019623,47.3216360168057,48.3193098316492,
49.3169836464926,50.3146574613361,51.3123312761795,52.310005091023,53.3076789058664,
54.3053527207099,55.3030265355533,56.3007003503968,57.2983741652402,58.2960479800837,
59.2937217949271,60.2913956097706,61.289069424614,62.2867432394575,63.2844170543009,
64.2820908691444,65.2797646839878,66.2774384988313,67.2751123136747,68.2727861285182,
69.2704599433616,70.2681337582051,71.2658075730485,72.263481387892,73.2611552027354,
74.2588290175789,75.2565028324223,76.2541766472658,77.2518504621092,78.2495242769527,
79.2471980917962),.UNSPECIFIED.);
#243=B_SPLINE_SURFACE_WITH_KNOTS('',3,3,((#11373,#11374,#11375,#11376,#11377,
#11378,#11379,#11380,#11381,#11382,#11383,#11384,#11385,#11386,#11387,#11388,
#11389,#11390,#11391,#11392,#11393,#11394,#11395,#11396,#11397,#11398,#11399,
#11400,#11401,#11402,#11403,#11404,#11405,#11406,#11407,#11408,#11409,#11410,
#11411,#11412,#11413,#11414,#11415,#11416,#11417,#11418,#11419,#11420,#11421,
#11422,#11423,#11424,#11425,#11426,#11427,#11428,#11429,#11430,#11431,#11432,
#11433,#11434,#11435,#11436,#11437,#11438,#11439,#11440),(#11441,#11442,
#11443,#11444,#11445,#11446,#11447,#11448,#11449,#11450,#11451,#11452,#11453,
#11454,#11455,#11456,#11457,#11458,#11459,#11460,#11461,#11462,#11463,#11464,
#11465,#11466,#11467,#11468,#11469,#11470,#11471,#11472,#11473,#11474,#11475,
#11476,#11477,#11478,#11479,#11480,#11481,#11482,#11483,#11484,#11485,#11486,
#11487,#11488,#11489,#11490,#11491,#11492,#11493,#11494,#11495,#11496,#11497,
#11498,#11499,#11500,#11501,#11502,#11503,#11504,#11505,#11506,#11507,#11508),
(#11509,#11510,#11511,#11512,#11513,#11514,#11515,#11516,#11517,#11518,
#11519,#11520,#11521,#11522,#11523,#11524,#11525,#11526,#11527,#11528,#11529,
#11530,#11531,#11532,#11533,#11534,#11535,#11536,#11537,#11538,#11539,#11540,
#11541,#11542,#11543,#11544,#11545,#11546,#11547,#11548,#11549,#11550,#11551,
#11552,#11553,#11554,#11555,#11556,#11557,#11558,#11559,#11560,#11561,#11562,
#11563,#11564,#11565,#11566,#11567,#11568,#11569,#11570,#11571,#11572,#11573,
#11574,#11575,#11576),(#11577,#11578,#11579,#11580,#11581,#11582,#11583,
#11584,#11585,#11586,#11587,#11588,#11589,#11590,#11591,#11592,#11593,#11594,
#11595,#11596,#11597,#11598,#11599,#11600,#11601,#11602,#11603,#11604,#11605,
#11606,#11607,#11608,#11609,#11610,#11611,#11612,#11613,#11614,#11615,#11616,
#11617,#11618,#11619,#11620,#11621,#11622,#11623,#11624,#11625,#11626,#11627,
#11628,#11629,#11630,#11631,#11632,#11633,#11634,#11635,#11636,#11637,#11638,
#11639,#11640,#11641,#11642,#11643,#11644)),.UNSPECIFIED.,.F.,.F.,.F.,(4,
4),(4,1,1,1,1,1,1,1,1,1,1,1,1,1,1,1,1,1,1,1,1,1,1,1,1,1,1,1,1,1,1,1,1,1,
1,1,1,1,1,1,1,1,1,1,1,1,1,1,1,1,1,1,1,1,1,1,1,1,1,1,1,1,1,1,1,4),(0.,0.0642013499338865),
(11.8589888623078,12.8566626771512,13.8543364919947,14.8520103068381,15.8496841216816,
16.847357936525,17.8450317513685,18.8427055662119,19.8403793810554,20.8380531958988,
21.8357270107423,22.8334008255857,23.8310746404292,24.8287484552726,25.8264222701161,
26.8240960849595,27.821769899803,28.8194437146464,29.8171175294899,30.8147913443333,
31.8124651591768,32.8101389740202,33.8078127888637,34.8054866037072,35.8031604185506,
36.8008342333941,37.7985080482375,38.796181863081,39.7938556779244,40.7915294927679,
41.7892033076113,42.7868771224548,43.7845509372982,44.7822247521417,45.7798985669851,
46.7775723818286,47.775246196672,48.7729200115155,49.7705938263589,50.7682676412024,
51.7659414560458,52.7636152708893,53.7612890857327,54.7589629005762,55.7566367154196,
56.7543105302631,57.7519843451065,58.74965815995,59.7473319747934,60.7450057896369,
61.7426796044803,62.7403534193238,63.7380272341672,64.7357010490107,65.7333748638541,
66.7310486786976,67.728722493541,68.7263963083845,69.7240701232279,70.7217439380714,
71.7194177529148,72.7170915677583,73.7147653826017,74.7124391974452,75.7101130122886,
76.7077868271321),.UNSPECIFIED.);
#244=B_SPLINE_SURFACE_WITH_KNOTS('',3,3,((#11764,#11765,#11766,#11767,#11768,
#11769,#11770,#11771,#11772,#11773,#11774,#11775,#11776,#11777,#11778,#11779,
#11780,#11781,#11782,#11783,#11784,#11785,#11786,#11787,#11788,#11789,#11790,
#11791,#11792,#11793,#11794,#11795,#11796,#11797,#11798,#11799,#11800,#11801,
#11802,#11803,#11804,#11805,#11806,#11807,#11808,#11809,#11810,#11811,#11812,
#11813,#11814,#11815,#11816,#11817,#11818,#11819,#11820,#11821,#11822,#11823,
#11824,#11825,#11826,#11827,#11828,#11829,#11830,#11831),(#11832,#11833,
#11834,#11835,#11836,#11837,#11838,#11839,#11840,#11841,#11842,#11843,#11844,
#11845,#11846,#11847,#11848,#11849,#11850,#11851,#11852,#11853,#11854,#11855,
#11856,#11857,#11858,#11859,#11860,#11861,#11862,#11863,#11864,#11865,#11866,
#11867,#11868,#11869,#11870,#11871,#11872,#11873,#11874,#11875,#11876,#11877,
#11878,#11879,#11880,#11881,#11882,#11883,#11884,#11885,#11886,#11887,#11888,
#11889,#11890,#11891,#11892,#11893,#11894,#11895,#11896,#11897,#11898,#11899),
(#11900,#11901,#11902,#11903,#11904,#11905,#11906,#11907,#11908,#11909,
#11910,#11911,#11912,#11913,#11914,#11915,#11916,#11917,#11918,#11919,#11920,
#11921,#11922,#11923,#11924,#11925,#11926,#11927,#11928,#11929,#11930,#11931,
#11932,#11933,#11934,#11935,#11936,#11937,#11938,#11939,#11940,#11941,#11942,
#11943,#11944,#11945,#11946,#11947,#11948,#11949,#11950,#11951,#11952,#11953,
#11954,#11955,#11956,#11957,#11958,#11959,#11960,#11961,#11962,#11963,#11964,
#11965,#11966,#11967),(#11968,#11969,#11970,#11971,#11972,#11973,#11974,
#11975,#11976,#11977,#11978,#11979,#11980,#11981,#11982,#11983,#11984,#11985,
#11986,#11987,#11988,#11989,#11990,#11991,#11992,#11993,#11994,#11995,#11996,
#11997,#11998,#11999,#12000,#12001,#12002,#12003,#12004,#12005,#12006,#12007,
#12008,#12009,#12010,#12011,#12012,#12013,#12014,#12015,#12016,#12017,#12018,
#12019,#12020,#12021,#12022,#12023,#12024,#12025,#12026,#12027,#12028,#12029,
#12030,#12031,#12032,#12033,#12034,#12035)),.UNSPECIFIED.,.F.,.F.,.F.,(4,
4),(4,1,1,1,1,1,1,1,1,1,1,1,1,1,1,1,1,1,1,1,1,1,1,1,1,1,1,1,1,1,1,1,1,1,
1,1,1,1,1,1,1,1,1,1,1,1,1,1,1,1,1,1,1,1,1,1,1,1,1,1,1,1,1,1,1,4),(0.,0.0642013499338865),
(14.3984001269718,15.3960739418153,16.3937477566587,17.3914215715022,18.3890953863456,
19.3867692011891,20.3844430160325,21.382116830876,22.3797906457194,23.3774644605629,
24.3751382754063,25.3728120902498,26.3704859050932,27.3681597199367,28.3658335347801,
29.3635073496236,30.361181164467,31.3588549793105,32.3565287941539,33.3542026089974,
34.3518764238408,35.3495502386843,36.3472240535277,37.3448978683712,38.3425716832146,
39.3402454980581,40.3379193129015,41.335593127745,42.3332669425884,43.3309407574319,
44.3286145722753,45.3262883871188,46.3239622019622,47.3216360168057,48.3193098316492,
49.3169836464926,50.3146574613361,51.3123312761795,52.310005091023,53.3076789058664,
54.3053527207099,55.3030265355533,56.3007003503968,57.2983741652402,58.2960479800837,
59.2937217949271,60.2913956097706,61.289069424614,62.2867432394575,63.2844170543009,
64.2820908691444,65.2797646839878,66.2774384988313,67.2751123136747,68.2727861285182,
69.2704599433616,70.2681337582051,71.2658075730485,72.263481387892,73.2611552027354,
74.2588290175789,75.2565028324223,76.2541766472658,77.2518504621092,78.2495242769527,
79.2471980917961),.UNSPECIFIED.);
#245=B_SPLINE_SURFACE_WITH_KNOTS('',3,3,((#12177,#12178,#12179,#12180,#12181,
#12182,#12183,#12184,#12185,#12186,#12187,#12188,#12189,#12190,#12191,#12192,
#12193,#12194,#12195,#12196,#12197,#12198,#12199,#12200,#12201,#12202,#12203,
#12204,#12205,#12206,#12207,#12208,#12209,#12210,#12211,#12212,#12213,#12214,
#12215,#12216,#12217,#12218,#12219,#12220,#12221,#12222,#12223,#12224,#12225,
#12226,#12227,#12228,#12229,#12230,#12231,#12232,#12233,#12234,#12235,#12236,
#12237,#12238,#12239,#12240,#12241,#12242,#12243,#12244),(#12245,#12246,
#12247,#12248,#12249,#12250,#12251,#12252,#12253,#12254,#12255,#12256,#12257,
#12258,#12259,#12260,#12261,#12262,#12263,#12264,#12265,#12266,#12267,#12268,
#12269,#12270,#12271,#12272,#12273,#12274,#12275,#12276,#12277,#12278,#12279,
#12280,#12281,#12282,#12283,#12284,#12285,#12286,#12287,#12288,#12289,#12290,
#12291,#12292,#12293,#12294,#12295,#12296,#12297,#12298,#12299,#12300,#12301,
#12302,#12303,#12304,#12305,#12306,#12307,#12308,#12309,#12310,#12311,#12312),
(#12313,#12314,#12315,#12316,#12317,#12318,#12319,#12320,#12321,#12322,
#12323,#12324,#12325,#12326,#12327,#12328,#12329,#12330,#12331,#12332,#12333,
#12334,#12335,#12336,#12337,#12338,#12339,#12340,#12341,#12342,#12343,#12344,
#12345,#12346,#12347,#12348,#12349,#12350,#12351,#12352,#12353,#12354,#12355,
#12356,#12357,#12358,#12359,#12360,#12361,#12362,#12363,#12364,#12365,#12366,
#12367,#12368,#12369,#12370,#12371,#12372,#12373,#12374,#12375,#12376,#12377,
#12378,#12379,#12380),(#12381,#12382,#12383,#12384,#12385,#12386,#12387,
#12388,#12389,#12390,#12391,#12392,#12393,#12394,#12395,#12396,#12397,#12398,
#12399,#12400,#12401,#12402,#12403,#12404,#12405,#12406,#12407,#12408,#12409,
#12410,#12411,#12412,#12413,#12414,#12415,#12416,#12417,#12418,#12419,#12420,
#12421,#12422,#12423,#12424,#12425,#12426,#12427,#12428,#12429,#12430,#12431,
#12432,#12433,#12434,#12435,#12436,#12437,#12438,#12439,#12440,#12441,#12442,
#12443,#12444,#12445,#12446,#12447,#12448)),.UNSPECIFIED.,.F.,.F.,.F.,(4,
4),(4,1,1,1,1,1,1,1,1,1,1,1,1,1,1,1,1,1,1,1,1,1,1,1,1,1,1,1,1,1,1,1,1,1,
1,1,1,1,1,1,1,1,1,1,1,1,1,1,1,1,1,1,1,1,1,1,1,1,1,1,1,1,1,1,1,4),(0.,0.0642013499338865),
(11.8589888623078,12.8566626771512,13.8543364919947,14.8520103068381,15.8496841216816,
16.8473579365251,17.8450317513685,18.842705566212,19.8403793810554,20.8380531958989,
21.8357270107423,22.8334008255858,23.8310746404292,24.8287484552727,25.8264222701161,
26.8240960849596,27.821769899803,28.8194437146465,29.8171175294899,30.8147913443334,
31.8124651591768,32.8101389740203,33.8078127888637,34.8054866037072,35.8031604185506,
36.8008342333941,37.7985080482375,38.796181863081,39.7938556779244,40.7915294927679,
41.7892033076113,42.7868771224548,43.7845509372982,44.7822247521417,45.7798985669851,
46.7775723818286,47.775246196672,48.7729200115155,49.7705938263589,50.7682676412024,
51.7659414560458,52.7636152708893,53.7612890857327,54.7589629005762,55.7566367154196,
56.7543105302631,57.7519843451065,58.74965815995,59.7473319747934,60.7450057896369,
61.7426796044803,62.7403534193238,63.7380272341672,64.7357010490107,65.7333748638542,
66.7310486786976,67.728722493541,68.7263963083845,69.7240701232279,70.7217439380714,
71.7194177529149,72.7170915677583,73.7147653826018,74.7124391974452,75.7101130122887,
76.7077868271321),.UNSPECIFIED.);
#246=B_SPLINE_SURFACE_WITH_KNOTS('',3,3,((#12568,#12569,#12570,#12571,#12572,
#12573,#12574,#12575,#12576,#12577,#12578,#12579,#12580,#12581,#12582,#12583,
#12584,#12585,#12586,#12587,#12588,#12589,#12590,#12591,#12592,#12593,#12594,
#12595,#12596,#12597,#12598,#12599,#12600,#12601,#12602,#12603,#12604,#12605,
#12606,#12607,#12608,#12609,#12610,#12611,#12612,#12613,#12614,#12615,#12616,
#12617,#12618,#12619,#12620,#12621,#12622,#12623,#12624,#12625,#12626,#12627,
#12628,#12629,#12630,#12631,#12632,#12633,#12634,#12635),(#12636,#12637,
#12638,#12639,#12640,#12641,#12642,#12643,#12644,#12645,#12646,#12647,#12648,
#12649,#12650,#12651,#12652,#12653,#12654,#12655,#12656,#12657,#12658,#12659,
#12660,#12661,#12662,#12663,#12664,#12665,#12666,#12667,#12668,#12669,#12670,
#12671,#12672,#12673,#12674,#12675,#12676,#12677,#12678,#12679,#12680,#12681,
#12682,#12683,#12684,#12685,#12686,#12687,#12688,#12689,#12690,#12691,#12692,
#12693,#12694,#12695,#12696,#12697,#12698,#12699,#12700,#12701,#12702,#12703),
(#12704,#12705,#12706,#12707,#12708,#12709,#12710,#12711,#12712,#12713,
#12714,#12715,#12716,#12717,#12718,#12719,#12720,#12721,#12722,#12723,#12724,
#12725,#12726,#12727,#12728,#12729,#12730,#12731,#12732,#12733,#12734,#12735,
#12736,#12737,#12738,#12739,#12740,#12741,#12742,#12743,#12744,#12745,#12746,
#12747,#12748,#12749,#12750,#12751,#12752,#12753,#12754,#12755,#12756,#12757,
#12758,#12759,#12760,#12761,#12762,#12763,#12764,#12765,#12766,#12767,#12768,
#12769,#12770,#12771),(#12772,#12773,#12774,#12775,#12776,#12777,#12778,
#12779,#12780,#12781,#12782,#12783,#12784,#12785,#12786,#12787,#12788,#12789,
#12790,#12791,#12792,#12793,#12794,#12795,#12796,#12797,#12798,#12799,#12800,
#12801,#12802,#12803,#12804,#12805,#12806,#12807,#12808,#12809,#12810,#12811,
#12812,#12813,#12814,#12815,#12816,#12817,#12818,#12819,#12820,#12821,#12822,
#12823,#12824,#12825,#12826,#12827,#12828,#12829,#12830,#12831,#12832,#12833,
#12834,#12835,#12836,#12837,#12838,#12839)),.UNSPECIFIED.,.F.,.F.,.F.,(4,
4),(4,1,1,1,1,1,1,1,1,1,1,1,1,1,1,1,1,1,1,1,1,1,1,1,1,1,1,1,1,1,1,1,1,1,
1,1,1,1,1,1,1,1,1,1,1,1,1,1,1,1,1,1,1,1,1,1,1,1,1,1,1,1,1,1,1,4),(0.,0.0642013499338865),
(14.3984001269718,15.3960739418153,16.3937477566587,17.3914215715022,18.3890953863456,
19.3867692011891,20.3844430160325,21.382116830876,22.3797906457194,23.3774644605629,
24.3751382754063,25.3728120902498,26.3704859050932,27.3681597199367,28.3658335347801,
29.3635073496236,30.361181164467,31.3588549793105,32.3565287941539,33.3542026089974,
34.3518764238408,35.3495502386843,36.3472240535278,37.3448978683712,38.3425716832147,
39.3402454980581,40.3379193129016,41.335593127745,42.3332669425885,43.3309407574319,
44.3286145722754,45.3262883871188,46.3239622019623,47.3216360168057,48.3193098316492,
49.3169836464926,50.3146574613361,51.3123312761795,52.310005091023,53.3076789058664,
54.3053527207099,55.3030265355533,56.3007003503968,57.2983741652402,58.2960479800837,
59.2937217949271,60.2913956097706,61.289069424614,62.2867432394575,63.2844170543009,
64.2820908691444,65.2797646839878,66.2774384988313,67.2751123136747,68.2727861285182,
69.2704599433616,70.2681337582051,71.2658075730485,72.263481387892,73.2611552027354,
74.2588290175789,75.2565028324223,76.2541766472658,77.2518504621092,78.2495242769527,
79.2471980917962),.UNSPECIFIED.);
#247=B_SPLINE_CURVE_WITH_KNOTS('',3,(#6191,#6192,#6193,#6194),
 .UNSPECIFIED.,.F.,.F.,(4,4),(64.141416212773,64.8487979648243),
 .UNSPECIFIED.);
#248=B_SPLINE_CURVE_WITH_KNOTS('',3,(#6197,#6198,#6199,#6200,#6201,#6202,
#6203,#6204,#6205,#6206),.UNSPECIFIED.,.F.,.F.,(4,3,3,4),(-62.8318530717959,
-61.855776520294,-60.8581027054505,-60.3976421702574),.UNSPECIFIED.);
#249=B_SPLINE_CURVE_WITH_KNOTS('',3,(#6211,#6212,#6213,#6214,#6215,#6216,
#6217,#6218,#6219,#6220,#6221,#6222,#6223,#6224,#6225,#6226,#6227,#6228,
#6229,#6230,#6231,#6232,#6233,#6234,#6235),.UNSPECIFIED.,.F.,.F.,(4,3,3,
3,3,3,3,3,4),(57.8582309055934,57.8650812609202,58.8627550757636,59.8604288906071,
60.8581027054505,61.855776520294,62.8534503351374,63.8511241499809,64.141416212773),
 .UNSPECIFIED.);
#250=B_SPLINE_CURVE_WITH_KNOTS('',3,(#6236,#6237,#6238,#6239,#6240,#6241,
#6242,#6243,#6244,#6245,#6246,#6247,#6248,#6249,#6250,#6251,#6252,#6253,
#6254,#6255,#6256,#6257),.UNSPECIFIED.,.F.,.F.,(4,3,3,3,3,3,3,4),(-60.3976421702574,
-59.8604288906071,-58.8627550757636,-57.8650812609202,-56.8674074460767,
-55.8697336312333,-54.8720598163898,-54.1144568630778),.UNSPECIFIED.);
#251=B_SPLINE_CURVE_WITH_KNOTS('',3,(#6262,#6263,#6264,#6265,#6266,#6267,
#6268,#6269,#6270,#6271,#6272,#6273,#6274,#6275,#6276,#6277,#6278,#6279,
#6280,#6281,#6282,#6283),.UNSPECIFIED.,.F.,.F.,(4,3,3,3,3,3,3,4),(51.5750455984138,
51.8790383718595,52.8767121867029,53.8743860015464,54.8720598163898,55.8697336312333,
56.8674074460767,57.8582309055934),.UNSPECIFIED.);
#252=B_SPLINE_CURVE_WITH_KNOTS('',3,(#6284,#6285,#6286,#6287,#6288,#6289,
#6290,#6291,#6292,#6293,#6294,#6295,#6296,#6297,#6298,#6299,#6300,#6301,
#6302,#6303,#6304,#6305,#6306,#6307,#6308),.UNSPECIFIED.,.F.,.F.,(4,3,3,
3,3,3,3,3,4),(-54.1144568630778,-53.8743860015464,-52.8767121867029,-51.8790383718595,
-50.881364557016,-49.8836907421726,-48.8860169273291,-47.8883431124856,
-47.8312715558982),.UNSPECIFIED.);
#253=B_SPLINE_CURVE_WITH_KNOTS('',3,(#6313,#6314,#6315,#6316,#6317,#6318,
#6319,#6320,#6321,#6322,#6323,#6324,#6325,#6326,#6327,#6328,#6329,#6330,
#6331,#6332,#6333,#6334),.UNSPECIFIED.,.F.,.F.,(4,3,3,3,3,3,3,4),(45.2918602912342,
45.8929954827987,46.8906692976422,47.8883431124856,48.8860169273291,49.8836907421726,
50.881364557016,51.5750455984138),.UNSPECIFIED.);
#254=B_SPLINE_CURVE_WITH_KNOTS('',3,(#6335,#6336,#6337,#6338,#6339,#6340,
#6341,#6342,#6343,#6344,#6345,#6346,#6347,#6348,#6349,#6350,#6351,#6352,
#6353,#6354,#6355,#6356),.UNSPECIFIED.,.F.,.F.,(4,3,3,3,3,3,3,4),(-47.8312715558982,
-46.8906692976422,-45.8929954827987,-44.8953216679553,-43.8976478531118,
-42.8999740382684,-41.9023002234249,-41.5480862487187),.UNSPECIFIED.);
#255=B_SPLINE_CURVE_WITH_KNOTS('',3,(#6361,#6362,#6363,#6364,#6365,#6366,
#6367,#6368,#6369,#6370,#6371,#6372,#6373,#6374,#6375,#6376,#6377,#6378,
#6379,#6380,#6381,#6382),.UNSPECIFIED.,.F.,.F.,(4,3,3,3,3,3,3,4),(39.0086749840546,
39.906952593738,40.9046264085815,41.9023002234249,42.8999740382684,43.8976478531118,
44.8953216679553,45.2918602912342),.UNSPECIFIED.);
#256=B_SPLINE_CURVE_WITH_KNOTS('',3,(#6383,#6384,#6385,#6386,#6387,#6388,
#6389,#6390,#6391,#6392,#6393,#6394,#6395,#6396,#6397,#6398,#6399,#6400,
#6401,#6402,#6403,#6404),.UNSPECIFIED.,.F.,.F.,(4,3,3,3,3,3,3,4),(-41.5480862487187,
-40.9046264085815,-39.906952593738,-38.9092787788946,-37.9116049640511,
-36.9139311492077,-35.9162573343642,-35.2649009415391),.UNSPECIFIED.);
#257=B_SPLINE_CURVE_WITH_KNOTS('',3,(#6409,#6410,#6411,#6412,#6413,#6414,
#6415,#6416,#6417,#6418,#6419,#6420,#6421,#6422,#6423,#6424,#6425,#6426,
#6427,#6428,#6429,#6430,#6431,#6432,#6433),.UNSPECIFIED.,.F.,.F.,(4,3,3,
3,3,3,3,3,4),(32.725489676875,32.9232358898339,33.9209097046773,34.9185835195208,
35.9162573343642,36.9139311492077,37.9116049640511,38.9092787788946,39.0086749840546),
 .UNSPECIFIED.);
#258=B_SPLINE_CURVE_WITH_KNOTS('',3,(#6434,#6435,#6436,#6437,#6438,#6439,
#6440,#6441,#6442,#6443,#6444,#6445,#6446,#6447,#6448,#6449,#6450,#6451,
#6452,#6453,#6454,#6455),.UNSPECIFIED.,.F.,.F.,(4,3,3,3,3,3,3,4),(-35.2649009415391,
-34.9185835195208,-33.9209097046773,-32.9232358898339,-31.9255620749904,
-30.927888260147,-29.9302144453035,-28.9817156343595),.UNSPECIFIED.);
#259=B_SPLINE_CURVE_WITH_KNOTS('',3,(#6460,#6461,#6462,#6463,#6464,#6465,
#6466,#6467,#6468,#6469,#6470,#6471,#6472,#6473,#6474,#6475,#6476,#6477,
#6478,#6479,#6480,#6481),.UNSPECIFIED.,.F.,.F.,(4,3,3,3,3,3,3,4),(26.4423043696954,
26.9371930007732,27.9348668156166,28.9325406304601,29.9302144453035,30.927888260147,
31.9255620749904,32.725489676875),.UNSPECIFIED.);
#260=B_SPLINE_CURVE_WITH_KNOTS('',3,(#6482,#6483,#6484,#6485,#6486,#6487,
#6488,#6489,#6490,#6491,#6492,#6493,#6494,#6495,#6496,#6497,#6498,#6499,
#6500,#6501,#6502,#6503,#6504,#6505,#6506),.UNSPECIFIED.,.F.,.F.,(4,3,3,
3,3,3,3,3,4),(-28.9817156343595,-28.9325406304601,-27.9348668156166,-26.9371930007732,
-25.9395191859297,-24.9418453710863,-23.9441715562428,-22.9464977413994,
-22.6985303271799),.UNSPECIFIED.);
#261=B_SPLINE_CURVE_WITH_KNOTS('',3,(#6511,#6512,#6513,#6514,#6515,#6516,
#6517,#6518,#6519,#6520,#6521,#6522,#6523,#6524,#6525,#6526,#6527,#6528,
#6529,#6530,#6531,#6532),.UNSPECIFIED.,.F.,.F.,(4,3,3,3,3,3,3,4),(20.1591190625158,
20.9511501117125,21.9488239265559,22.9464977413994,23.9441715562428,24.9418453710863,
25.9395191859297,26.4423043696954),.UNSPECIFIED.);
#262=B_SPLINE_CURVE_WITH_KNOTS('',3,(#6533,#6534,#6535,#6536,#6537,#6538,
#6539,#6540,#6541,#6542,#6543,#6544,#6545,#6546,#6547,#6548,#6549,#6550,
#6551,#6552,#6553,#6554),.UNSPECIFIED.,.F.,.F.,(4,3,3,3,3,3,3,4),(-22.6985303271799,
-21.9488239265559,-20.9511501117125,-19.953476296869,-18.9558024820256,
-17.9581286671821,-16.9604548523387,-16.4153450200003),.UNSPECIFIED.);
#263=B_SPLINE_CURVE_WITH_KNOTS('',3,(#6559,#6560,#6561,#6562,#6563,#6564,
#6565,#6566,#6567,#6568,#6569,#6570,#6571,#6572,#6573,#6574,#6575,#6576,
#6577,#6578,#6579,#6580,#6581,#6582,#6583),.UNSPECIFIED.,.F.,.F.,(4,3,3,
3,3,3,3,3,4),(13.8759337553362,13.9674334078083,14.9651072226518,15.9627810374952,
16.9604548523387,17.9581286671821,18.9558024820256,19.953476296869,20.1591190625158),
 .UNSPECIFIED.);
#264=B_SPLINE_CURVE_WITH_KNOTS('',3,(#6584,#6585,#6586,#6587,#6588,#6589,
#6590,#6591,#6592,#6593,#6594,#6595,#6596,#6597,#6598,#6599,#6600,#6601,
#6602,#6603,#6604,#6605),.UNSPECIFIED.,.F.,.F.,(4,3,3,3,3,3,3,4),(-16.4153450200003,
-15.9627810374952,-14.9651072226518,-13.9674334078083,-12.9697595929649,
-11.9720857781214,-10.974411963278,-10.1321597128207),.UNSPECIFIED.);
#265=B_SPLINE_CURVE_WITH_KNOTS('',3,(#6611,#6612,#6613,#6614,#6615,#6616,
#6617,#6618,#6619,#6620,#6621,#6622,#6623),.UNSPECIFIED.,.F.,.F.,(4,3,3,
3,4),(-3.84897440564113,-2.99302144453035,-1.99534762968691,-0.997673814843449,
0.),.UNSPECIFIED.);
#266=B_SPLINE_CURVE_WITH_KNOTS('',3,(#6626,#6627,#6628,#6629,#6630,#6631,
#6632,#6633,#6634,#6635,#6636,#6637,#6638,#6639,#6640,#6641,#6642,#6643,
#6644),.UNSPECIFIED.,.F.,.F.,(4,3,3,3,3,3,4),(2.01694489302844,2.99302144453035,
3.9906952593738,4.98836907421725,5.9860428890607,6.98371670390416,7.59274844815664),
 .UNSPECIFIED.);
#267=B_SPLINE_CURVE_WITH_KNOTS('',3,(#6650,#6651,#6652,#6653),
 .UNSPECIFIED.,.F.,.F.,(4,4),(64.141416212773,64.8487979648243),
 .UNSPECIFIED.);
#268=B_SPLINE_CURVE_WITH_KNOTS('',3,(#6656,#6657,#6658,#6659,#6660,#6661,
#6662,#6663,#6664,#6665),.UNSPECIFIED.,.F.,.F.,(4,3,3,4),(-62.8318530717958,
-61.855776520294,-60.8581027054505,-60.3976421702575),.UNSPECIFIED.);
#269=B_SPLINE_CURVE_WITH_KNOTS('',3,(#6670,#6671,#6672,#6673,#6674,#6675,
#6676,#6677,#6678,#6679,#6680,#6681,#6682,#6683,#6684,#6685,#6686,#6687,
#6688,#6689,#6690,#6691,#6692,#6693,#6694),.UNSPECIFIED.,.F.,.F.,(4,3,3,
3,3,3,3,3,4),(57.8582309055934,57.8650812609202,58.8627550757636,59.8604288906071,
60.8581027054505,61.855776520294,62.8534503351374,63.8511241499808,64.141416212773),
 .UNSPECIFIED.);
#270=B_SPLINE_CURVE_WITH_KNOTS('',3,(#6695,#6696,#6697,#6698,#6699,#6700,
#6701,#6702,#6703,#6704,#6705,#6706,#6707,#6708,#6709,#6710,#6711,#6712,
#6713,#6714,#6715,#6716),.UNSPECIFIED.,.F.,.F.,(4,3,3,3,3,3,3,4),(-60.3976421702575,
-59.8604288906071,-58.8627550757636,-57.8650812609201,-56.8674074460767,
-55.8697336312333,-54.8720598163898,-54.1144568630779),.UNSPECIFIED.);
#271=B_SPLINE_CURVE_WITH_KNOTS('',3,(#6721,#6722,#6723,#6724,#6725,#6726,
#6727,#6728,#6729,#6730,#6731,#6732,#6733,#6734,#6735,#6736,#6737,#6738,
#6739,#6740,#6741,#6742),.UNSPECIFIED.,.F.,.F.,(4,3,3,3,3,3,3,4),(51.5750455984138,
51.8790383718595,52.8767121867029,53.8743860015464,54.8720598163898,55.8697336312333,
56.8674074460767,57.8582309055934),.UNSPECIFIED.);
#272=B_SPLINE_CURVE_WITH_KNOTS('',3,(#6743,#6744,#6745,#6746,#6747,#6748,
#6749,#6750,#6751,#6752,#6753,#6754,#6755,#6756,#6757,#6758,#6759,#6760,
#6761,#6762,#6763,#6764,#6765,#6766,#6767),.UNSPECIFIED.,.F.,.F.,(4,3,3,
3,3,3,3,3,4),(-54.1144568630779,-53.8743860015464,-52.8767121867029,-51.8790383718595,
-50.881364557016,-49.8836907421726,-48.8860169273291,-47.8883431124857,
-47.8312715558983),.UNSPECIFIED.);
#273=B_SPLINE_CURVE_WITH_KNOTS('',3,(#6772,#6773,#6774,#6775,#6776,#6777,
#6778,#6779,#6780,#6781,#6782,#6783,#6784,#6785,#6786,#6787,#6788,#6789,
#6790,#6791,#6792,#6793),.UNSPECIFIED.,.F.,.F.,(4,3,3,3,3,3,3,4),(45.2918602912342,
45.8929954827987,46.8906692976422,47.8883431124857,48.8860169273291,49.8836907421725,
50.881364557016,51.5750455984138),.UNSPECIFIED.);
#274=B_SPLINE_CURVE_WITH_KNOTS('',3,(#6794,#6795,#6796,#6797,#6798,#6799,
#6800,#6801,#6802,#6803,#6804,#6805,#6806,#6807,#6808,#6809,#6810,#6811,
#6812,#6813,#6814,#6815),.UNSPECIFIED.,.F.,.F.,(4,3,3,3,3,3,3,4),(-47.8312715558983,
-46.8906692976422,-45.8929954827987,-44.8953216679553,-43.8976478531118,
-42.8999740382684,-41.9023002234249,-41.5480862487187),.UNSPECIFIED.);
#275=B_SPLINE_CURVE_WITH_KNOTS('',3,(#6820,#6821,#6822,#6823,#6824,#6825,
#6826,#6827,#6828,#6829,#6830,#6831,#6832,#6833,#6834,#6835,#6836,#6837,
#6838,#6839,#6840,#6841),.UNSPECIFIED.,.F.,.F.,(4,3,3,3,3,3,3,4),(39.0086749840546,
39.906952593738,40.9046264085815,41.9023002234249,42.8999740382684,43.8976478531118,
44.8953216679553,45.2918602912342),.UNSPECIFIED.);
#276=B_SPLINE_CURVE_WITH_KNOTS('',3,(#6842,#6843,#6844,#6845,#6846,#6847,
#6848,#6849,#6850,#6851,#6852,#6853,#6854,#6855,#6856,#6857,#6858,#6859,
#6860,#6861,#6862,#6863),.UNSPECIFIED.,.F.,.F.,(4,3,3,3,3,3,3,4),(-41.5480862487187,
-40.9046264085815,-39.906952593738,-38.9092787788946,-37.9116049640511,
-36.9139311492077,-35.9162573343642,-35.2649009415391),.UNSPECIFIED.);
#277=B_SPLINE_CURVE_WITH_KNOTS('',3,(#6868,#6869,#6870,#6871,#6872,#6873,
#6874,#6875,#6876,#6877,#6878,#6879,#6880,#6881,#6882,#6883,#6884,#6885,
#6886,#6887,#6888,#6889,#6890,#6891,#6892),.UNSPECIFIED.,.F.,.F.,(4,3,3,
3,3,3,3,3,4),(32.725489676875,32.9232358898339,33.9209097046773,34.9185835195208,
35.9162573343642,36.9139311492077,37.9116049640511,38.9092787788946,39.0086749840546),
 .UNSPECIFIED.);
#278=B_SPLINE_CURVE_WITH_KNOTS('',3,(#6893,#6894,#6895,#6896,#6897,#6898,
#6899,#6900,#6901,#6902,#6903,#6904,#6905,#6906,#6907,#6908,#6909,#6910,
#6911,#6912,#6913,#6914),.UNSPECIFIED.,.F.,.F.,(4,3,3,3,3,3,3,4),(-35.2649009415391,
-34.9185835195208,-33.9209097046773,-32.9232358898339,-31.9255620749904,
-30.927888260147,-29.9302144453035,-28.9817156343595),.UNSPECIFIED.);
#279=B_SPLINE_CURVE_WITH_KNOTS('',3,(#6919,#6920,#6921,#6922,#6923,#6924,
#6925,#6926,#6927,#6928,#6929,#6930,#6931,#6932,#6933,#6934,#6935,#6936,
#6937,#6938,#6939,#6940),.UNSPECIFIED.,.F.,.F.,(4,3,3,3,3,3,3,4),(26.4423043696954,
26.9371930007732,27.9348668156166,28.9325406304601,29.9302144453035,30.927888260147,
31.9255620749904,32.725489676875),.UNSPECIFIED.);
#280=B_SPLINE_CURVE_WITH_KNOTS('',3,(#6941,#6942,#6943,#6944,#6945,#6946,
#6947,#6948,#6949,#6950,#6951,#6952,#6953,#6954,#6955,#6956,#6957,#6958,
#6959,#6960,#6961,#6962,#6963,#6964,#6965),.UNSPECIFIED.,.F.,.F.,(4,3,3,
3,3,3,3,3,4),(-28.9817156343595,-28.9325406304601,-27.9348668156166,-26.9371930007732,
-25.9395191859297,-24.9418453710863,-23.9441715562428,-22.9464977413994,
-22.6985303271799),.UNSPECIFIED.);
#281=B_SPLINE_CURVE_WITH_KNOTS('',3,(#6970,#6971,#6972,#6973,#6974,#6975,
#6976,#6977,#6978,#6979,#6980,#6981,#6982,#6983,#6984,#6985,#6986,#6987,
#6988,#6989,#6990,#6991),.UNSPECIFIED.,.F.,.F.,(4,3,3,3,3,3,3,4),(20.1591190625158,
20.9511501117125,21.9488239265559,22.9464977413994,23.9441715562428,24.9418453710863,
25.9395191859297,26.4423043696954),.UNSPECIFIED.);
#282=B_SPLINE_CURVE_WITH_KNOTS('',3,(#6992,#6993,#6994,#6995,#6996,#6997,
#6998,#6999,#7000,#7001,#7002,#7003,#7004,#7005,#7006,#7007,#7008,#7009,
#7010,#7011,#7012,#7013),.UNSPECIFIED.,.F.,.F.,(4,3,3,3,3,3,3,4),(-22.6985303271799,
-21.9488239265559,-20.9511501117125,-19.953476296869,-18.9558024820256,
-17.9581286671821,-16.9604548523387,-16.4153450200003),.UNSPECIFIED.);
#283=B_SPLINE_CURVE_WITH_KNOTS('',3,(#7018,#7019,#7020,#7021,#7022,#7023,
#7024,#7025,#7026,#7027,#7028,#7029,#7030,#7031,#7032,#7033,#7034,#7035,
#7036,#7037,#7038,#7039,#7040,#7041,#7042),.UNSPECIFIED.,.F.,.F.,(4,3,3,
3,3,3,3,3,4),(13.8759337553362,13.9674334078083,14.9651072226518,15.9627810374952,
16.9604548523387,17.9581286671821,18.9558024820256,19.953476296869,20.1591190625158),
 .UNSPECIFIED.);
#284=B_SPLINE_CURVE_WITH_KNOTS('',3,(#7043,#7044,#7045,#7046,#7047,#7048,
#7049,#7050,#7051,#7052,#7053,#7054,#7055,#7056,#7057,#7058,#7059,#7060,
#7061,#7062,#7063,#7064),.UNSPECIFIED.,.F.,.F.,(4,3,3,3,3,3,3,4),(-16.4153450200003,
-15.9627810374952,-14.9651072226518,-13.9674334078083,-12.9697595929649,
-11.9720857781214,-10.974411963278,-10.1321597128207),.UNSPECIFIED.);
#285=B_SPLINE_CURVE_WITH_KNOTS('',3,(#7070,#7071,#7072,#7073,#7074,#7075,
#7076,#7077,#7078,#7079,#7080,#7081,#7082),.UNSPECIFIED.,.F.,.F.,(4,3,3,
3,4),(-3.84897440564115,-2.99302144453035,-1.9953476296869,-0.997673814843451,
0.),.UNSPECIFIED.);
#286=B_SPLINE_CURVE_WITH_KNOTS('',3,(#7085,#7086,#7087,#7088,#7089,#7090,
#7091,#7092,#7093,#7094,#7095,#7096,#7097,#7098,#7099,#7100,#7101,#7102,
#7103),.UNSPECIFIED.,.F.,.F.,(4,3,3,3,3,3,4),(2.0169448930285,2.99302144453035,
3.99069525937381,4.98836907421726,5.98604288906071,6.98371670390416,7.59274844815666),
 .UNSPECIFIED.);
#287=B_SPLINE_CURVE_WITH_KNOTS('',3,(#7109,#7110,#7111,#7112),
 .UNSPECIFIED.,.F.,.F.,(4,4),(64.141416212773,64.8487979648243),
 .UNSPECIFIED.);
#288=B_SPLINE_CURVE_WITH_KNOTS('',3,(#7115,#7116,#7117,#7118,#7119,#7120,
#7121,#7122,#7123,#7124),.UNSPECIFIED.,.F.,.F.,(4,3,3,4),(-62.8318530717958,
-61.855776520294,-60.8581027054505,-60.3976421702574),.UNSPECIFIED.);
#289=B_SPLINE_CURVE_WITH_KNOTS('',3,(#7129,#7130,#7131,#7132,#7133,#7134,
#7135,#7136,#7137,#7138,#7139,#7140,#7141,#7142,#7143,#7144,#7145,#7146,
#7147,#7148,#7149,#7150,#7151,#7152,#7153),.UNSPECIFIED.,.F.,.F.,(4,3,3,
3,3,3,3,3,4),(57.8582309055934,57.8650812609202,58.8627550757636,59.8604288906071,
60.8581027054505,61.855776520294,62.8534503351374,63.8511241499808,64.141416212773),
 .UNSPECIFIED.);
#290=B_SPLINE_CURVE_WITH_KNOTS('',3,(#7154,#7155,#7156,#7157,#7158,#7159,
#7160,#7161,#7162,#7163,#7164,#7165,#7166,#7167,#7168,#7169,#7170,#7171,
#7172,#7173,#7174,#7175),.UNSPECIFIED.,.F.,.F.,(4,3,3,3,3,3,3,4),(-60.3976421702574,
-59.8604288906071,-58.8627550757636,-57.8650812609202,-56.8674074460767,
-55.8697336312333,-54.8720598163898,-54.1144568630778),.UNSPECIFIED.);
#291=B_SPLINE_CURVE_WITH_KNOTS('',3,(#7180,#7181,#7182,#7183,#7184,#7185,
#7186,#7187,#7188,#7189,#7190,#7191,#7192,#7193,#7194,#7195,#7196,#7197,
#7198,#7199,#7200,#7201),.UNSPECIFIED.,.F.,.F.,(4,3,3,3,3,3,3,4),(51.5750455984138,
51.8790383718595,52.8767121867029,53.8743860015464,54.8720598163898,55.8697336312333,
56.8674074460767,57.8582309055934),.UNSPECIFIED.);
#292=B_SPLINE_CURVE_WITH_KNOTS('',3,(#7202,#7203,#7204,#7205,#7206,#7207,
#7208,#7209,#7210,#7211,#7212,#7213,#7214,#7215,#7216,#7217,#7218,#7219,
#7220,#7221,#7222,#7223,#7224,#7225,#7226),.UNSPECIFIED.,.F.,.F.,(4,3,3,
3,3,3,3,3,4),(-54.1144568630778,-53.8743860015464,-52.8767121867029,-51.8790383718595,
-50.881364557016,-49.8836907421726,-48.8860169273291,-47.8883431124856,
-47.8312715558982),.UNSPECIFIED.);
#293=B_SPLINE_CURVE_WITH_KNOTS('',3,(#7231,#7232,#7233,#7234,#7235,#7236,
#7237,#7238,#7239,#7240,#7241,#7242,#7243,#7244,#7245,#7246,#7247,#7248,
#7249,#7250,#7251,#7252),.UNSPECIFIED.,.F.,.F.,(4,3,3,3,3,3,3,4),(45.2918602912342,
45.8929954827987,46.8906692976422,47.8883431124856,48.8860169273291,49.8836907421725,
50.881364557016,51.5750455984138),.UNSPECIFIED.);
#294=B_SPLINE_CURVE_WITH_KNOTS('',3,(#7253,#7254,#7255,#7256,#7257,#7258,
#7259,#7260,#7261,#7262,#7263,#7264,#7265,#7266,#7267,#7268,#7269,#7270,
#7271,#7272,#7273,#7274),.UNSPECIFIED.,.F.,.F.,(4,3,3,3,3,3,3,4),(-47.8312715558982,
-46.8906692976422,-45.8929954827987,-44.8953216679553,-43.8976478531118,
-42.8999740382684,-41.9023002234249,-41.5480862487187),.UNSPECIFIED.);
#295=B_SPLINE_CURVE_WITH_KNOTS('',3,(#7279,#7280,#7281,#7282,#7283,#7284,
#7285,#7286,#7287,#7288,#7289,#7290,#7291,#7292,#7293,#7294,#7295,#7296,
#7297,#7298,#7299,#7300),.UNSPECIFIED.,.F.,.F.,(4,3,3,3,3,3,3,4),(39.0086749840546,
39.906952593738,40.9046264085815,41.9023002234249,42.8999740382684,43.8976478531118,
44.8953216679553,45.2918602912342),.UNSPECIFIED.);
#296=B_SPLINE_CURVE_WITH_KNOTS('',3,(#7301,#7302,#7303,#7304,#7305,#7306,
#7307,#7308,#7309,#7310,#7311,#7312,#7313,#7314,#7315,#7316,#7317,#7318,
#7319,#7320,#7321,#7322),.UNSPECIFIED.,.F.,.F.,(4,3,3,3,3,3,3,4),(-41.5480862487187,
-40.9046264085815,-39.906952593738,-38.9092787788946,-37.9116049640511,
-36.9139311492077,-35.9162573343642,-35.2649009415391),.UNSPECIFIED.);
#297=B_SPLINE_CURVE_WITH_KNOTS('',3,(#7327,#7328,#7329,#7330,#7331,#7332,
#7333,#7334,#7335,#7336,#7337,#7338,#7339,#7340,#7341,#7342,#7343,#7344,
#7345,#7346,#7347,#7348,#7349,#7350,#7351),.UNSPECIFIED.,.F.,.F.,(4,3,3,
3,3,3,3,3,4),(32.725489676875,32.9232358898339,33.9209097046773,34.9185835195208,
35.9162573343642,36.9139311492077,37.9116049640511,38.9092787788946,39.0086749840546),
 .UNSPECIFIED.);
#298=B_SPLINE_CURVE_WITH_KNOTS('',3,(#7352,#7353,#7354,#7355,#7356,#7357,
#7358,#7359,#7360,#7361,#7362,#7363,#7364,#7365,#7366,#7367,#7368,#7369,
#7370,#7371,#7372,#7373),.UNSPECIFIED.,.F.,.F.,(4,3,3,3,3,3,3,4),(-35.2649009415391,
-34.9185835195208,-33.9209097046773,-32.9232358898339,-31.9255620749904,
-30.927888260147,-29.9302144453035,-28.9817156343595),.UNSPECIFIED.);
#299=B_SPLINE_CURVE_WITH_KNOTS('',3,(#7378,#7379,#7380,#7381,#7382,#7383,
#7384,#7385,#7386,#7387,#7388,#7389,#7390,#7391,#7392,#7393,#7394,#7395,
#7396,#7397,#7398,#7399),.UNSPECIFIED.,.F.,.F.,(4,3,3,3,3,3,3,4),(26.4423043696954,
26.9371930007732,27.9348668156166,28.9325406304601,29.9302144453035,30.927888260147,
31.9255620749904,32.725489676875),.UNSPECIFIED.);
#300=B_SPLINE_CURVE_WITH_KNOTS('',3,(#7400,#7401,#7402,#7403,#7404,#7405,
#7406,#7407,#7408,#7409,#7410,#7411,#7412,#7413,#7414,#7415,#7416,#7417,
#7418,#7419,#7420,#7421,#7422,#7423,#7424),.UNSPECIFIED.,.F.,.F.,(4,3,3,
3,3,3,3,3,4),(-28.9817156343595,-28.9325406304601,-27.9348668156166,-26.9371930007732,
-25.9395191859297,-24.9418453710863,-23.9441715562428,-22.9464977413994,
-22.6985303271799),.UNSPECIFIED.);
#301=B_SPLINE_CURVE_WITH_KNOTS('',3,(#7429,#7430,#7431,#7432,#7433,#7434,
#7435,#7436,#7437,#7438,#7439,#7440,#7441,#7442,#7443,#7444,#7445,#7446,
#7447,#7448,#7449,#7450),.UNSPECIFIED.,.F.,.F.,(4,3,3,3,3,3,3,4),(20.1591190625158,
20.9511501117125,21.9488239265559,22.9464977413994,23.9441715562428,24.9418453710863,
25.9395191859297,26.4423043696954),.UNSPECIFIED.);
#302=B_SPLINE_CURVE_WITH_KNOTS('',3,(#7451,#7452,#7453,#7454,#7455,#7456,
#7457,#7458,#7459,#7460,#7461,#7462,#7463,#7464,#7465,#7466,#7467,#7468,
#7469,#7470,#7471,#7472),.UNSPECIFIED.,.F.,.F.,(4,3,3,3,3,3,3,4),(-22.6985303271799,
-21.9488239265559,-20.9511501117125,-19.953476296869,-18.9558024820256,
-17.9581286671821,-16.9604548523387,-16.4153450200003),.UNSPECIFIED.);
#303=B_SPLINE_CURVE_WITH_KNOTS('',3,(#7477,#7478,#7479,#7480,#7481,#7482,
#7483,#7484,#7485,#7486,#7487,#7488,#7489,#7490,#7491,#7492,#7493,#7494,
#7495,#7496,#7497,#7498,#7499,#7500,#7501),.UNSPECIFIED.,.F.,.F.,(4,3,3,
3,3,3,3,3,4),(13.8759337553362,13.9674334078083,14.9651072226518,15.9627810374952,
16.9604548523387,17.9581286671821,18.9558024820256,19.953476296869,20.1591190625158),
 .UNSPECIFIED.);
#304=B_SPLINE_CURVE_WITH_KNOTS('',3,(#7502,#7503,#7504,#7505,#7506,#7507,
#7508,#7509,#7510,#7511,#7512,#7513,#7514,#7515,#7516,#7517,#7518,#7519,
#7520,#7521,#7522,#7523),.UNSPECIFIED.,.F.,.F.,(4,3,3,3,3,3,3,4),(-16.4153450200003,
-15.9627810374952,-14.9651072226518,-13.9674334078083,-12.9697595929649,
-11.9720857781214,-10.974411963278,-10.1321597128207),.UNSPECIFIED.);
#305=B_SPLINE_CURVE_WITH_KNOTS('',3,(#7529,#7530,#7531,#7532,#7533,#7534,
#7535,#7536,#7537,#7538,#7539,#7540,#7541),.UNSPECIFIED.,.F.,.F.,(4,3,3,
3,4),(-3.84897440564114,-2.99302144453035,-1.9953476296869,-0.997673814843452,
0.),.UNSPECIFIED.);
#306=B_SPLINE_CURVE_WITH_KNOTS('',3,(#7544,#7545,#7546,#7547,#7548,#7549,
#7550,#7551,#7552,#7553,#7554,#7555,#7556,#7557,#7558,#7559,#7560,#7561,
#7562),.UNSPECIFIED.,.F.,.F.,(4,3,3,3,3,3,4),(2.0169448930285,2.99302144453035,
3.9906952593738,4.98836907421725,5.9860428890607,6.98371670390415,7.59274844815666),
 .UNSPECIFIED.);
#307=B_SPLINE_CURVE_WITH_KNOTS('',3,(#7568,#7569,#7570,#7571),
 .UNSPECIFIED.,.F.,.F.,(4,4),(64.141416212773,64.8487979648243),
 .UNSPECIFIED.);
#308=B_SPLINE_CURVE_WITH_KNOTS('',3,(#7574,#7575,#7576,#7577,#7578,#7579,
#7580,#7581,#7582,#7583),.UNSPECIFIED.,.F.,.F.,(4,3,3,4),(-62.8318530717959,
-61.855776520294,-60.8581027054505,-60.3976421702574),.UNSPECIFIED.);
#309=B_SPLINE_CURVE_WITH_KNOTS('',3,(#7588,#7589,#7590,#7591,#7592,#7593,
#7594,#7595,#7596,#7597,#7598,#7599,#7600,#7601,#7602,#7603,#7604,#7605,
#7606,#7607,#7608,#7609,#7610,#7611,#7612),.UNSPECIFIED.,.F.,.F.,(4,3,3,
3,3,3,3,3,4),(57.8582309055934,57.8650812609202,58.8627550757636,59.8604288906071,
60.8581027054505,61.855776520294,62.8534503351374,63.8511241499808,64.141416212773),
 .UNSPECIFIED.);
#310=B_SPLINE_CURVE_WITH_KNOTS('',3,(#7613,#7614,#7615,#7616,#7617,#7618,
#7619,#7620,#7621,#7622,#7623,#7624,#7625,#7626,#7627,#7628,#7629,#7630,
#7631,#7632,#7633,#7634),.UNSPECIFIED.,.F.,.F.,(4,3,3,3,3,3,3,4),(-60.3976421702574,
-59.8604288906071,-58.8627550757636,-57.8650812609202,-56.8674074460767,
-55.8697336312333,-54.8720598163898,-54.1144568630778),.UNSPECIFIED.);
#311=B_SPLINE_CURVE_WITH_KNOTS('',3,(#7639,#7640,#7641,#7642,#7643,#7644,
#7645,#7646,#7647,#7648,#7649,#7650,#7651,#7652,#7653,#7654,#7655,#7656,
#7657,#7658,#7659,#7660),.UNSPECIFIED.,.F.,.F.,(4,3,3,3,3,3,3,4),(51.5750455984138,
51.8790383718595,52.8767121867029,53.8743860015464,54.8720598163898,55.8697336312333,
56.8674074460767,57.8582309055934),.UNSPECIFIED.);
#312=B_SPLINE_CURVE_WITH_KNOTS('',3,(#7661,#7662,#7663,#7664,#7665,#7666,
#7667,#7668,#7669,#7670,#7671,#7672,#7673,#7674,#7675,#7676,#7677,#7678,
#7679,#7680,#7681,#7682,#7683,#7684,#7685),.UNSPECIFIED.,.F.,.F.,(4,3,3,
3,3,3,3,3,4),(-54.1144568630778,-53.8743860015464,-52.8767121867029,-51.8790383718595,
-50.881364557016,-49.8836907421725,-48.8860169273291,-47.8883431124856,
-47.8312715558982),.UNSPECIFIED.);
#313=B_SPLINE_CURVE_WITH_KNOTS('',3,(#7690,#7691,#7692,#7693,#7694,#7695,
#7696,#7697,#7698,#7699,#7700,#7701,#7702,#7703,#7704,#7705,#7706,#7707,
#7708,#7709,#7710,#7711),.UNSPECIFIED.,.F.,.F.,(4,3,3,3,3,3,3,4),(45.2918602912342,
45.8929954827987,46.8906692976422,47.8883431124857,48.8860169273291,49.8836907421726,
50.881364557016,51.5750455984138),.UNSPECIFIED.);
#314=B_SPLINE_CURVE_WITH_KNOTS('',3,(#7712,#7713,#7714,#7715,#7716,#7717,
#7718,#7719,#7720,#7721,#7722,#7723,#7724,#7725,#7726,#7727,#7728,#7729,
#7730,#7731,#7732,#7733),.UNSPECIFIED.,.F.,.F.,(4,3,3,3,3,3,3,4),(-47.8312715558982,
-46.8906692976422,-45.8929954827987,-44.8953216679553,-43.8976478531118,
-42.8999740382684,-41.9023002234249,-41.5480862487187),.UNSPECIFIED.);
#315=B_SPLINE_CURVE_WITH_KNOTS('',3,(#7738,#7739,#7740,#7741,#7742,#7743,
#7744,#7745,#7746,#7747,#7748,#7749,#7750,#7751,#7752,#7753,#7754,#7755,
#7756,#7757,#7758,#7759),.UNSPECIFIED.,.F.,.F.,(4,3,3,3,3,3,3,4),(39.0086749840546,
39.906952593738,40.9046264085815,41.9023002234249,42.8999740382684,43.8976478531118,
44.8953216679553,45.2918602912342),.UNSPECIFIED.);
#316=B_SPLINE_CURVE_WITH_KNOTS('',3,(#7760,#7761,#7762,#7763,#7764,#7765,
#7766,#7767,#7768,#7769,#7770,#7771,#7772,#7773,#7774,#7775,#7776,#7777,
#7778,#7779,#7780,#7781),.UNSPECIFIED.,.F.,.F.,(4,3,3,3,3,3,3,4),(-41.5480862487187,
-40.9046264085815,-39.906952593738,-38.9092787788946,-37.9116049640511,
-36.9139311492077,-35.9162573343642,-35.2649009415391),.UNSPECIFIED.);
#317=B_SPLINE_CURVE_WITH_KNOTS('',3,(#7786,#7787,#7788,#7789,#7790,#7791,
#7792,#7793,#7794,#7795,#7796,#7797,#7798,#7799,#7800,#7801,#7802,#7803,
#7804,#7805,#7806,#7807,#7808,#7809,#7810),.UNSPECIFIED.,.F.,.F.,(4,3,3,
3,3,3,3,3,4),(32.725489676875,32.9232358898339,33.9209097046773,34.9185835195208,
35.9162573343642,36.9139311492077,37.9116049640511,38.9092787788946,39.0086749840546),
 .UNSPECIFIED.);
#318=B_SPLINE_CURVE_WITH_KNOTS('',3,(#7811,#7812,#7813,#7814,#7815,#7816,
#7817,#7818,#7819,#7820,#7821,#7822,#7823,#7824,#7825,#7826,#7827,#7828,
#7829,#7830,#7831,#7832),.UNSPECIFIED.,.F.,.F.,(4,3,3,3,3,3,3,4),(-35.2649009415391,
-34.9185835195208,-33.9209097046773,-32.9232358898339,-31.9255620749904,
-30.927888260147,-29.9302144453035,-28.9817156343595),.UNSPECIFIED.);
#319=B_SPLINE_CURVE_WITH_KNOTS('',3,(#7837,#7838,#7839,#7840,#7841,#7842,
#7843,#7844,#7845,#7846,#7847,#7848,#7849,#7850,#7851,#7852,#7853,#7854,
#7855,#7856,#7857,#7858),.UNSPECIFIED.,.F.,.F.,(4,3,3,3,3,3,3,4),(26.4423043696954,
26.9371930007732,27.9348668156166,28.9325406304601,29.9302144453035,30.927888260147,
31.9255620749904,32.725489676875),.UNSPECIFIED.);
#320=B_SPLINE_CURVE_WITH_KNOTS('',3,(#7859,#7860,#7861,#7862,#7863,#7864,
#7865,#7866,#7867,#7868,#7869,#7870,#7871,#7872,#7873,#7874,#7875,#7876,
#7877,#7878,#7879,#7880,#7881,#7882,#7883),.UNSPECIFIED.,.F.,.F.,(4,3,3,
3,3,3,3,3,4),(-28.9817156343595,-28.9325406304601,-27.9348668156166,-26.9371930007732,
-25.9395191859297,-24.9418453710863,-23.9441715562428,-22.9464977413994,
-22.6985303271799),.UNSPECIFIED.);
#321=B_SPLINE_CURVE_WITH_KNOTS('',3,(#7888,#7889,#7890,#7891,#7892,#7893,
#7894,#7895,#7896,#7897,#7898,#7899,#7900,#7901,#7902,#7903,#7904,#7905,
#7906,#7907,#7908,#7909),.UNSPECIFIED.,.F.,.F.,(4,3,3,3,3,3,3,4),(20.1591190625158,
20.9511501117125,21.9488239265559,22.9464977413994,23.9441715562428,24.9418453710863,
25.9395191859297,26.4423043696954),.UNSPECIFIED.);
#322=B_SPLINE_CURVE_WITH_KNOTS('',3,(#7910,#7911,#7912,#7913,#7914,#7915,
#7916,#7917,#7918,#7919,#7920,#7921,#7922,#7923,#7924,#7925,#7926,#7927,
#7928,#7929,#7930,#7931),.UNSPECIFIED.,.F.,.F.,(4,3,3,3,3,3,3,4),(-22.6985303271799,
-21.9488239265559,-20.9511501117125,-19.953476296869,-18.9558024820256,
-17.9581286671821,-16.9604548523387,-16.4153450200003),.UNSPECIFIED.);
#323=B_SPLINE_CURVE_WITH_KNOTS('',3,(#7936,#7937,#7938,#7939,#7940,#7941,
#7942,#7943,#7944,#7945,#7946,#7947,#7948,#7949,#7950,#7951,#7952,#7953,
#7954,#7955,#7956,#7957,#7958,#7959,#7960),.UNSPECIFIED.,.F.,.F.,(4,3,3,
3,3,3,3,3,4),(13.8759337553362,13.9674334078083,14.9651072226518,15.9627810374952,
16.9604548523387,17.9581286671821,18.9558024820256,19.953476296869,20.1591190625158),
 .UNSPECIFIED.);
#324=B_SPLINE_CURVE_WITH_KNOTS('',3,(#7961,#7962,#7963,#7964,#7965,#7966,
#7967,#7968,#7969,#7970,#7971,#7972,#7973,#7974,#7975,#7976,#7977,#7978,
#7979,#7980,#7981,#7982),.UNSPECIFIED.,.F.,.F.,(4,3,3,3,3,3,3,4),(-16.4153450200003,
-15.9627810374952,-14.9651072226518,-13.9674334078083,-12.9697595929649,
-11.9720857781214,-10.974411963278,-10.1321597128207),.UNSPECIFIED.);
#325=B_SPLINE_CURVE_WITH_KNOTS('',3,(#7988,#7989,#7990,#7991,#7992,#7993,
#7994,#7995,#7996,#7997,#7998,#7999,#8000),.UNSPECIFIED.,.F.,.F.,(4,3,3,
3,4),(-3.84897440564114,-2.99302144453035,-1.9953476296869,-0.997673814843451,
0.),.UNSPECIFIED.);
#326=B_SPLINE_CURVE_WITH_KNOTS('',3,(#8003,#8004,#8005,#8006,#8007,#8008,
#8009,#8010,#8011,#8012,#8013,#8014,#8015,#8016,#8017,#8018,#8019,#8020,
#8021),.UNSPECIFIED.,.F.,.F.,(4,3,3,3,3,3,4),(2.01694489302845,2.99302144453035,
3.9906952593738,4.98836907421725,5.98604288906071,6.98371670390416,7.59274844815666),
 .UNSPECIFIED.);
#327=B_SPLINE_CURVE_WITH_KNOTS('',3,(#8027,#8028,#8029,#8030,#8031,#8032,
#8033,#8034),.UNSPECIFIED.,.F.,.F.,(4,1,1,1,1,4),(72.2566310325652,72.7170915677583,
73.7147653826018,74.7124391974452,75.7101130122887,76.7077868271321),
 .UNSPECIFIED.);
#328=B_SPLINE_CURVE_WITH_KNOTS('',3,(#8037,#8038,#8039,#8040,#8041,#8042,
#8043,#8044,#8045),.UNSPECIFIED.,.F.,.F.,(4,1,1,1,1,1,4),(72.2566310325652,
72.263481387892,73.2611552027354,74.2588290175789,75.2565028324223,76.2541766472658,
77.2302531987677),.UNSPECIFIED.);
#329=B_SPLINE_CURVE_WITH_KNOTS('',3,(#8050,#8051,#8052,#8053,#8054,#8055,
#8056,#8057,#8058,#8059),.UNSPECIFIED.,.F.,.F.,(4,1,1,1,1,1,1,4),(65.9734457253856,
66.7310486786976,67.728722493541,68.7263963083845,69.7240701232279,70.7217439380714,
71.7194177529149,72.2566310325652),.UNSPECIFIED.);
#330=B_SPLINE_CURVE_WITH_KNOTS('',3,(#8060,#8061,#8062,#8063,#8064,#8065,
#8066,#8067,#8068,#8069),.UNSPECIFIED.,.F.,.F.,(4,1,1,1,1,1,1,4),(65.9734457253856,
66.2774384988313,67.2751123136747,68.2727861285182,69.2704599433616,70.2681337582051,
71.2658075730485,72.2566310325652),.UNSPECIFIED.);
#331=B_SPLINE_CURVE_WITH_KNOTS('',3,(#8074,#8075,#8076,#8077,#8078,#8079,
#8080,#8081,#8082,#8083,#8084),.UNSPECIFIED.,.F.,.F.,(4,1,1,1,1,1,1,1,4),
(59.6902604182061,59.7473319747934,60.7450057896369,61.7426796044803,62.7403534193238,
63.7380272341672,64.7357010490107,65.7333748638542,65.9734457253856),
 .UNSPECIFIED.);
#332=B_SPLINE_CURVE_WITH_KNOTS('',3,(#8085,#8086,#8087,#8088,#8089,#8090,
#8091,#8092,#8093,#8094),.UNSPECIFIED.,.F.,.F.,(4,1,1,1,1,1,1,4),(59.6902604182061,
60.2913956097706,61.289069424614,62.2867432394575,63.2844170543009,64.2820908691444,
65.2797646839878,65.9734457253856),.UNSPECIFIED.);
#333=B_SPLINE_CURVE_WITH_KNOTS('',3,(#8099,#8100,#8101,#8102,#8103,#8104,
#8105,#8106,#8107,#8108),.UNSPECIFIED.,.F.,.F.,(4,1,1,1,1,1,1,4),(53.4070751110265,
53.7612890857327,54.7589629005762,55.7566367154196,56.7543105302631,57.7519843451065,
58.74965815995,59.6902604182061),.UNSPECIFIED.);
#334=B_SPLINE_CURVE_WITH_KNOTS('',3,(#8109,#8110,#8111,#8112,#8113,#8114,
#8115,#8116,#8117,#8118),.UNSPECIFIED.,.F.,.F.,(4,1,1,1,1,1,1,4),(53.4070751110265,
54.3053527207099,55.3030265355533,56.3007003503968,57.2983741652402,58.2960479800837,
59.2937217949271,59.6902604182061),.UNSPECIFIED.);
#335=B_SPLINE_CURVE_WITH_KNOTS('',3,(#8123,#8124,#8125,#8126,#8127,#8128,
#8129,#8130,#8131,#8132),.UNSPECIFIED.,.F.,.F.,(4,1,1,1,1,1,1,4),(47.1238898038469,
47.775246196672,48.7729200115155,49.7705938263589,50.7682676412024,51.7659414560458,
52.7636152708893,53.4070751110265),.UNSPECIFIED.);
#336=B_SPLINE_CURVE_WITH_KNOTS('',3,(#8133,#8134,#8135,#8136,#8137,#8138,
#8139,#8140,#8141,#8142,#8143),.UNSPECIFIED.,.F.,.F.,(4,1,1,1,1,1,1,1,4),
(47.1238898038469,47.3216360168057,48.3193098316492,49.3169836464926,50.3146574613361,
51.3123312761795,52.310005091023,53.3076789058664,53.4070751110265),
 .UNSPECIFIED.);
#337=B_SPLINE_CURVE_WITH_KNOTS('',3,(#8148,#8149,#8150,#8151,#8152,#8153,
#8154,#8155,#8156,#8157),.UNSPECIFIED.,.F.,.F.,(4,1,1,1,1,1,1,4),(40.8407044966673,
41.7892033076113,42.7868771224548,43.7845509372982,44.7822247521417,45.7798985669851,
46.7775723818286,47.1238898038469),.UNSPECIFIED.);
#338=B_SPLINE_CURVE_WITH_KNOTS('',3,(#8158,#8159,#8160,#8161,#8162,#8163,
#8164,#8165,#8166,#8167),.UNSPECIFIED.,.F.,.F.,(4,1,1,1,1,1,1,4),(40.8407044966673,
41.335593127745,42.3332669425885,43.3309407574319,44.3286145722754,45.3262883871188,
46.3239622019623,47.1238898038469),.UNSPECIFIED.);
#339=B_SPLINE_CURVE_WITH_KNOTS('',3,(#8172,#8173,#8174,#8175,#8176,#8177,
#8178,#8179,#8180,#8181,#8182),.UNSPECIFIED.,.F.,.F.,(4,1,1,1,1,1,1,1,4),
(34.5575191894877,34.8054866037072,35.8031604185506,36.8008342333941,37.7985080482375,
38.796181863081,39.7938556779244,40.7915294927679,40.8407044966673),
 .UNSPECIFIED.);
#340=B_SPLINE_CURVE_WITH_KNOTS('',3,(#8183,#8184,#8185,#8186,#8187,#8188,
#8189,#8190,#8191,#8192),.UNSPECIFIED.,.F.,.F.,(4,1,1,1,1,1,1,4),(34.5575191894877,
35.3495502386843,36.3472240535278,37.3448978683712,38.3425716832147,39.3402454980581,
40.3379193129016,40.8407044966673),.UNSPECIFIED.);
#341=B_SPLINE_CURVE_WITH_KNOTS('',3,(#8197,#8198,#8199,#8200,#8201,#8202,
#8203,#8204,#8205,#8206),.UNSPECIFIED.,.F.,.F.,(4,1,1,1,1,1,1,4),(28.2743338823081,
28.8194437146465,29.8171175294899,30.8147913443334,31.8124651591768,32.8101389740203,
33.8078127888637,34.5575191894877),.UNSPECIFIED.);
#342=B_SPLINE_CURVE_WITH_KNOTS('',3,(#8207,#8208,#8209,#8210,#8211,#8212,
#8213,#8214,#8215,#8216,#8217),.UNSPECIFIED.,.F.,.F.,(4,1,1,1,1,1,1,1,4),
(28.2743338823081,28.3658335347801,29.3635073496236,30.361181164467,31.3588549793105,
32.3565287941539,33.3542026089974,34.3518764238408,34.5575191894877),
 .UNSPECIFIED.);
#343=B_SPLINE_CURVE_WITH_KNOTS('',3,(#8222,#8223,#8224,#8225,#8226,#8227,
#8228,#8229,#8230,#8231),.UNSPECIFIED.,.F.,.F.,(4,1,1,1,1,1,1,4),(21.9911485751285,
22.8334008255858,23.8310746404292,24.8287484552727,25.8264222701161,26.8240960849596,
27.821769899803,28.2743338823081),.UNSPECIFIED.);
#344=B_SPLINE_CURVE_WITH_KNOTS('',3,(#8232,#8233,#8234,#8235,#8236,#8237,
#8238,#8239,#8240,#8241),.UNSPECIFIED.,.F.,.F.,(4,1,1,1,1,1,1,4),(21.9911485751285,
22.3797906457194,23.3774644605629,24.3751382754063,25.3728120902498,26.3704859050932,
27.3681597199367,28.2743338823081),.UNSPECIFIED.);
#345=B_SPLINE_CURVE_WITH_KNOTS('',3,(#8247,#8248,#8249,#8250,#8251),
 .UNSPECIFIED.,.F.,.F.,(4,1,4),(14.3984001269718,15.3960739418153,15.7079632679489),
 .UNSPECIFIED.);
#346=B_SPLINE_CURVE_WITH_KNOTS('',3,(#8254,#8255,#8256,#8257,#8258),
 .UNSPECIFIED.,.F.,.F.,(4,1,4),(13.8759337553362,14.8520103068381,15.7079632679489),
 .UNSPECIFIED.);
#347=B_SPLINE_CURVE_WITH_KNOTS('',3,(#8264,#8265,#8266,#8267,#8268,#8269,
#8270,#8271),.UNSPECIFIED.,.F.,.F.,(4,1,1,1,1,4),(72.2566310325652,72.7170915677583,
73.7147653826017,74.7124391974452,75.7101130122886,76.7077868271321),
 .UNSPECIFIED.);
#348=B_SPLINE_CURVE_WITH_KNOTS('',3,(#8274,#8275,#8276,#8277,#8278,#8279,
#8280,#8281,#8282),.UNSPECIFIED.,.F.,.F.,(4,1,1,1,1,1,4),(72.2566310325652,
72.263481387892,73.2611552027354,74.2588290175789,75.2565028324223,76.2541766472658,
77.2302531987677),.UNSPECIFIED.);
#349=B_SPLINE_CURVE_WITH_KNOTS('',3,(#8287,#8288,#8289,#8290,#8291,#8292,
#8293,#8294,#8295,#8296),.UNSPECIFIED.,.F.,.F.,(4,1,1,1,1,1,1,4),(65.9734457253856,
66.7310486786976,67.728722493541,68.7263963083845,69.7240701232279,70.7217439380714,
71.7194177529148,72.2566310325652),.UNSPECIFIED.);
#350=B_SPLINE_CURVE_WITH_KNOTS('',3,(#8297,#8298,#8299,#8300,#8301,#8302,
#8303,#8304,#8305,#8306),.UNSPECIFIED.,.F.,.F.,(4,1,1,1,1,1,1,4),(65.9734457253856,
66.2774384988313,67.2751123136747,68.2727861285182,69.2704599433616,70.2681337582051,
71.2658075730485,72.2566310325652),.UNSPECIFIED.);
#351=B_SPLINE_CURVE_WITH_KNOTS('',3,(#8311,#8312,#8313,#8314,#8315,#8316,
#8317,#8318,#8319,#8320,#8321),.UNSPECIFIED.,.F.,.F.,(4,1,1,1,1,1,1,1,4),
(59.6902604182061,59.7473319747934,60.7450057896369,61.7426796044803,62.7403534193238,
63.7380272341672,64.7357010490107,65.7333748638541,65.9734457253856),
 .UNSPECIFIED.);
#352=B_SPLINE_CURVE_WITH_KNOTS('',3,(#8322,#8323,#8324,#8325,#8326,#8327,
#8328,#8329,#8330,#8331),.UNSPECIFIED.,.F.,.F.,(4,1,1,1,1,1,1,4),(59.6902604182061,
60.2913956097706,61.289069424614,62.2867432394575,63.2844170543009,64.2820908691444,
65.2797646839878,65.9734457253856),.UNSPECIFIED.);
#353=B_SPLINE_CURVE_WITH_KNOTS('',3,(#8336,#8337,#8338,#8339,#8340,#8341,
#8342,#8343,#8344,#8345),.UNSPECIFIED.,.F.,.F.,(4,1,1,1,1,1,1,4),(53.4070751110265,
53.7612890857327,54.7589629005762,55.7566367154196,56.7543105302631,57.7519843451065,
58.74965815995,59.6902604182061),.UNSPECIFIED.);
#354=B_SPLINE_CURVE_WITH_KNOTS('',3,(#8346,#8347,#8348,#8349,#8350,#8351,
#8352,#8353,#8354,#8355),.UNSPECIFIED.,.F.,.F.,(4,1,1,1,1,1,1,4),(53.4070751110265,
54.3053527207099,55.3030265355533,56.3007003503968,57.2983741652402,58.2960479800837,
59.2937217949271,59.6902604182061),.UNSPECIFIED.);
#355=B_SPLINE_CURVE_WITH_KNOTS('',3,(#8360,#8361,#8362,#8363,#8364,#8365,
#8366,#8367,#8368,#8369),.UNSPECIFIED.,.F.,.F.,(4,1,1,1,1,1,1,4),(47.1238898038469,
47.775246196672,48.7729200115155,49.7705938263589,50.7682676412024,51.7659414560458,
52.7636152708893,53.4070751110265),.UNSPECIFIED.);
#356=B_SPLINE_CURVE_WITH_KNOTS('',3,(#8370,#8371,#8372,#8373,#8374,#8375,
#8376,#8377,#8378,#8379,#8380),.UNSPECIFIED.,.F.,.F.,(4,1,1,1,1,1,1,1,4),
(47.1238898038469,47.3216360168057,48.3193098316492,49.3169836464926,50.3146574613361,
51.3123312761795,52.310005091023,53.3076789058664,53.4070751110265),
 .UNSPECIFIED.);
#357=B_SPLINE_CURVE_WITH_KNOTS('',3,(#8385,#8386,#8387,#8388,#8389,#8390,
#8391,#8392,#8393,#8394),.UNSPECIFIED.,.F.,.F.,(4,1,1,1,1,1,1,4),(40.8407044966673,
41.7892033076113,42.7868771224548,43.7845509372982,44.7822247521417,45.7798985669851,
46.7775723818286,47.1238898038469),.UNSPECIFIED.);
#358=B_SPLINE_CURVE_WITH_KNOTS('',3,(#8395,#8396,#8397,#8398,#8399,#8400,
#8401,#8402,#8403,#8404),.UNSPECIFIED.,.F.,.F.,(4,1,1,1,1,1,1,4),(40.8407044966673,
41.335593127745,42.3332669425884,43.3309407574319,44.3286145722753,45.3262883871188,
46.3239622019622,47.1238898038469),.UNSPECIFIED.);
#359=B_SPLINE_CURVE_WITH_KNOTS('',3,(#8409,#8410,#8411,#8412,#8413,#8414,
#8415,#8416,#8417,#8418,#8419),.UNSPECIFIED.,.F.,.F.,(4,1,1,1,1,1,1,1,4),
(34.5575191894877,34.8054866037072,35.8031604185506,36.8008342333941,37.7985080482375,
38.796181863081,39.7938556779244,40.7915294927679,40.8407044966673),
 .UNSPECIFIED.);
#360=B_SPLINE_CURVE_WITH_KNOTS('',3,(#8420,#8421,#8422,#8423,#8424,#8425,
#8426,#8427,#8428,#8429),.UNSPECIFIED.,.F.,.F.,(4,1,1,1,1,1,1,4),(34.5575191894877,
35.3495502386843,36.3472240535277,37.3448978683712,38.3425716832146,39.3402454980581,
40.3379193129015,40.8407044966673),.UNSPECIFIED.);
#361=B_SPLINE_CURVE_WITH_KNOTS('',3,(#8434,#8435,#8436,#8437,#8438,#8439,
#8440,#8441,#8442,#8443),.UNSPECIFIED.,.F.,.F.,(4,1,1,1,1,1,1,4),(28.2743338823081,
28.8194437146464,29.8171175294899,30.8147913443333,31.8124651591768,32.8101389740202,
33.8078127888637,34.5575191894877),.UNSPECIFIED.);
#362=B_SPLINE_CURVE_WITH_KNOTS('',3,(#8444,#8445,#8446,#8447,#8448,#8449,
#8450,#8451,#8452,#8453,#8454),.UNSPECIFIED.,.F.,.F.,(4,1,1,1,1,1,1,1,4),
(28.2743338823081,28.3658335347801,29.3635073496236,30.361181164467,31.3588549793105,
32.3565287941539,33.3542026089974,34.3518764238408,34.5575191894877),
 .UNSPECIFIED.);
#363=B_SPLINE_CURVE_WITH_KNOTS('',3,(#8459,#8460,#8461,#8462,#8463,#8464,
#8465,#8466,#8467,#8468),.UNSPECIFIED.,.F.,.F.,(4,1,1,1,1,1,1,4),(21.9911485751285,
22.8334008255857,23.8310746404292,24.8287484552726,25.8264222701161,26.8240960849595,
27.821769899803,28.2743338823081),.UNSPECIFIED.);
#364=B_SPLINE_CURVE_WITH_KNOTS('',3,(#8469,#8470,#8471,#8472,#8473,#8474,
#8475,#8476,#8477,#8478),.UNSPECIFIED.,.F.,.F.,(4,1,1,1,1,1,1,4),(21.9911485751285,
22.3797906457194,23.3774644605629,24.3751382754063,25.3728120902498,26.3704859050932,
27.3681597199367,28.2743338823081),.UNSPECIFIED.);
#365=B_SPLINE_CURVE_WITH_KNOTS('',3,(#8484,#8485,#8486,#8487,#8488),
 .UNSPECIFIED.,.F.,.F.,(4,1,4),(14.3984001269718,15.3960739418153,15.7079632679489),
 .UNSPECIFIED.);
#366=B_SPLINE_CURVE_WITH_KNOTS('',3,(#8491,#8492,#8493,#8494,#8495),
 .UNSPECIFIED.,.F.,.F.,(4,1,4),(13.8759337553362,14.8520103068381,15.7079632679489),
 .UNSPECIFIED.);
#367=B_SPLINE_CURVE_WITH_KNOTS('',3,(#8501,#8502,#8503,#8504,#8505,#8506,
#8507,#8508),.UNSPECIFIED.,.F.,.F.,(4,1,1,1,1,4),(72.2566310325652,72.7170915677583,
73.7147653826018,74.7124391974452,75.7101130122887,76.7077868271321),
 .UNSPECIFIED.);
#368=B_SPLINE_CURVE_WITH_KNOTS('',3,(#8511,#8512,#8513,#8514,#8515,#8516,
#8517,#8518,#8519),.UNSPECIFIED.,.F.,.F.,(4,1,1,1,1,1,4),(72.2566310325652,
72.263481387892,73.2611552027354,74.2588290175789,75.2565028324223,76.2541766472658,
77.2302531987677),.UNSPECIFIED.);
#369=B_SPLINE_CURVE_WITH_KNOTS('',3,(#8524,#8525,#8526,#8527,#8528,#8529,
#8530,#8531,#8532,#8533),.UNSPECIFIED.,.F.,.F.,(4,1,1,1,1,1,1,4),(65.9734457253856,
66.7310486786976,67.728722493541,68.7263963083845,69.7240701232279,70.7217439380714,
71.7194177529149,72.2566310325652),.UNSPECIFIED.);
#370=B_SPLINE_CURVE_WITH_KNOTS('',3,(#8534,#8535,#8536,#8537,#8538,#8539,
#8540,#8541,#8542,#8543),.UNSPECIFIED.,.F.,.F.,(4,1,1,1,1,1,1,4),(65.9734457253856,
66.2774384988313,67.2751123136747,68.2727861285182,69.2704599433616,70.2681337582051,
71.2658075730485,72.2566310325652),.UNSPECIFIED.);
#371=B_SPLINE_CURVE_WITH_KNOTS('',3,(#8548,#8549,#8550,#8551,#8552,#8553,
#8554,#8555,#8556,#8557,#8558),.UNSPECIFIED.,.F.,.F.,(4,1,1,1,1,1,1,1,4),
(59.6902604182061,59.7473319747934,60.7450057896369,61.7426796044803,62.7403534193238,
63.7380272341672,64.7357010490107,65.7333748638542,65.9734457253856),
 .UNSPECIFIED.);
#372=B_SPLINE_CURVE_WITH_KNOTS('',3,(#8559,#8560,#8561,#8562,#8563,#8564,
#8565,#8566,#8567,#8568),.UNSPECIFIED.,.F.,.F.,(4,1,1,1,1,1,1,4),(59.6902604182061,
60.2913956097706,61.289069424614,62.2867432394575,63.2844170543009,64.2820908691444,
65.2797646839878,65.9734457253856),.UNSPECIFIED.);
#373=B_SPLINE_CURVE_WITH_KNOTS('',3,(#8573,#8574,#8575,#8576,#8577,#8578,
#8579,#8580,#8581,#8582),.UNSPECIFIED.,.F.,.F.,(4,1,1,1,1,1,1,4),(53.4070751110265,
53.7612890857327,54.7589629005762,55.7566367154196,56.7543105302631,57.7519843451065,
58.74965815995,59.6902604182061),.UNSPECIFIED.);
#374=B_SPLINE_CURVE_WITH_KNOTS('',3,(#8583,#8584,#8585,#8586,#8587,#8588,
#8589,#8590,#8591,#8592),.UNSPECIFIED.,.F.,.F.,(4,1,1,1,1,1,1,4),(53.4070751110265,
54.3053527207099,55.3030265355533,56.3007003503968,57.2983741652402,58.2960479800837,
59.2937217949271,59.6902604182061),.UNSPECIFIED.);
#375=B_SPLINE_CURVE_WITH_KNOTS('',3,(#8597,#8598,#8599,#8600,#8601,#8602,
#8603,#8604,#8605,#8606),.UNSPECIFIED.,.F.,.F.,(4,1,1,1,1,1,1,4),(47.1238898038469,
47.775246196672,48.7729200115155,49.7705938263589,50.7682676412024,51.7659414560458,
52.7636152708893,53.4070751110265),.UNSPECIFIED.);
#376=B_SPLINE_CURVE_WITH_KNOTS('',3,(#8607,#8608,#8609,#8610,#8611,#8612,
#8613,#8614,#8615,#8616,#8617),.UNSPECIFIED.,.F.,.F.,(4,1,1,1,1,1,1,1,4),
(47.1238898038469,47.3216360168057,48.3193098316492,49.3169836464926,50.3146574613361,
51.3123312761795,52.310005091023,53.3076789058664,53.4070751110265),
 .UNSPECIFIED.);
#377=B_SPLINE_CURVE_WITH_KNOTS('',3,(#8622,#8623,#8624,#8625,#8626,#8627,
#8628,#8629,#8630,#8631),.UNSPECIFIED.,.F.,.F.,(4,1,1,1,1,1,1,4),(40.8407044966673,
41.7892033076113,42.7868771224548,43.7845509372982,44.7822247521417,45.7798985669851,
46.7775723818286,47.1238898038469),.UNSPECIFIED.);
#378=B_SPLINE_CURVE_WITH_KNOTS('',3,(#8632,#8633,#8634,#8635,#8636,#8637,
#8638,#8639,#8640,#8641),.UNSPECIFIED.,.F.,.F.,(4,1,1,1,1,1,1,4),(40.8407044966673,
41.335593127745,42.3332669425885,43.3309407574319,44.3286145722754,45.3262883871188,
46.3239622019623,47.1238898038469),.UNSPECIFIED.);
#379=B_SPLINE_CURVE_WITH_KNOTS('',3,(#8646,#8647,#8648,#8649,#8650,#8651,
#8652,#8653,#8654,#8655,#8656),.UNSPECIFIED.,.F.,.F.,(4,1,1,1,1,1,1,1,4),
(34.5575191894877,34.8054866037072,35.8031604185506,36.8008342333941,37.7985080482375,
38.796181863081,39.7938556779244,40.7915294927679,40.8407044966673),
 .UNSPECIFIED.);
#380=B_SPLINE_CURVE_WITH_KNOTS('',3,(#8657,#8658,#8659,#8660,#8661,#8662,
#8663,#8664,#8665,#8666),.UNSPECIFIED.,.F.,.F.,(4,1,1,1,1,1,1,4),(34.5575191894877,
35.3495502386843,36.3472240535278,37.3448978683712,38.3425716832147,39.3402454980581,
40.3379193129016,40.8407044966673),.UNSPECIFIED.);
#381=B_SPLINE_CURVE_WITH_KNOTS('',3,(#8671,#8672,#8673,#8674,#8675,#8676,
#8677,#8678,#8679,#8680),.UNSPECIFIED.,.F.,.F.,(4,1,1,1,1,1,1,4),(28.2743338823081,
28.8194437146465,29.8171175294899,30.8147913443334,31.8124651591768,32.8101389740203,
33.8078127888637,34.5575191894877),.UNSPECIFIED.);
#382=B_SPLINE_CURVE_WITH_KNOTS('',3,(#8681,#8682,#8683,#8684,#8685,#8686,
#8687,#8688,#8689,#8690,#8691),.UNSPECIFIED.,.F.,.F.,(4,1,1,1,1,1,1,1,4),
(28.2743338823081,28.3658335347801,29.3635073496236,30.361181164467,31.3588549793105,
32.3565287941539,33.3542026089974,34.3518764238408,34.5575191894877),
 .UNSPECIFIED.);
#383=B_SPLINE_CURVE_WITH_KNOTS('',3,(#8696,#8697,#8698,#8699,#8700,#8701,
#8702,#8703,#8704,#8705),.UNSPECIFIED.,.F.,.F.,(4,1,1,1,1,1,1,4),(21.9911485751285,
22.8334008255858,23.8310746404292,24.8287484552727,25.8264222701161,26.8240960849596,
27.821769899803,28.2743338823081),.UNSPECIFIED.);
#384=B_SPLINE_CURVE_WITH_KNOTS('',3,(#8706,#8707,#8708,#8709,#8710,#8711,
#8712,#8713,#8714,#8715),.UNSPECIFIED.,.F.,.F.,(4,1,1,1,1,1,1,4),(21.9911485751285,
22.3797906457194,23.3774644605629,24.3751382754063,25.3728120902498,26.3704859050932,
27.3681597199367,28.2743338823081),.UNSPECIFIED.);
#385=B_SPLINE_CURVE_WITH_KNOTS('',3,(#8721,#8722,#8723,#8724,#8725),
 .UNSPECIFIED.,.F.,.F.,(4,1,4),(14.3984001269718,15.3960739418153,15.7079632679489),
 .UNSPECIFIED.);
#386=B_SPLINE_CURVE_WITH_KNOTS('',3,(#8728,#8729,#8730,#8731,#8732),
 .UNSPECIFIED.,.F.,.F.,(4,1,4),(13.8759337553362,14.8520103068381,15.7079632679489),
 .UNSPECIFIED.);
#387=B_SPLINE_CURVE_WITH_KNOTS('',3,(#8738,#8739,#8740,#8741,#8742,#8743,
#8744,#8745),.UNSPECIFIED.,.F.,.F.,(4,1,1,1,1,4),(72.2566310325652,72.7170915677583,
73.7147653826018,74.7124391974452,75.7101130122887,76.7077868271321),
 .UNSPECIFIED.);
#388=B_SPLINE_CURVE_WITH_KNOTS('',3,(#8748,#8749,#8750,#8751,#8752,#8753,
#8754,#8755,#8756),.UNSPECIFIED.,.F.,.F.,(4,1,1,1,1,1,4),(72.2566310325652,
72.263481387892,73.2611552027354,74.2588290175789,75.2565028324223,76.2541766472658,
77.2302531987677),.UNSPECIFIED.);
#389=B_SPLINE_CURVE_WITH_KNOTS('',3,(#8761,#8762,#8763,#8764,#8765,#8766,
#8767,#8768,#8769,#8770),.UNSPECIFIED.,.F.,.F.,(4,1,1,1,1,1,1,4),(65.9734457253856,
66.7310486786976,67.728722493541,68.7263963083845,69.7240701232279,70.7217439380714,
71.7194177529149,72.2566310325652),.UNSPECIFIED.);
#390=B_SPLINE_CURVE_WITH_KNOTS('',3,(#8771,#8772,#8773,#8774,#8775,#8776,
#8777,#8778,#8779,#8780),.UNSPECIFIED.,.F.,.F.,(4,1,1,1,1,1,1,4),(65.9734457253856,
66.2774384988313,67.2751123136747,68.2727861285182,69.2704599433616,70.2681337582051,
71.2658075730485,72.2566310325652),.UNSPECIFIED.);
#391=B_SPLINE_CURVE_WITH_KNOTS('',3,(#8785,#8786,#8787,#8788,#8789,#8790,
#8791,#8792,#8793,#8794,#8795),.UNSPECIFIED.,.F.,.F.,(4,1,1,1,1,1,1,1,4),
(59.6902604182061,59.7473319747934,60.7450057896369,61.7426796044803,62.7403534193238,
63.7380272341672,64.7357010490107,65.7333748638542,65.9734457253856),
 .UNSPECIFIED.);
#392=B_SPLINE_CURVE_WITH_KNOTS('',3,(#8796,#8797,#8798,#8799,#8800,#8801,
#8802,#8803,#8804,#8805),.UNSPECIFIED.,.F.,.F.,(4,1,1,1,1,1,1,4),(59.6902604182061,
60.2913956097706,61.289069424614,62.2867432394575,63.2844170543009,64.2820908691444,
65.2797646839878,65.9734457253856),.UNSPECIFIED.);
#393=B_SPLINE_CURVE_WITH_KNOTS('',3,(#8810,#8811,#8812,#8813,#8814,#8815,
#8816,#8817,#8818,#8819),.UNSPECIFIED.,.F.,.F.,(4,1,1,1,1,1,1,4),(53.4070751110265,
53.7612890857327,54.7589629005762,55.7566367154196,56.7543105302631,57.7519843451065,
58.74965815995,59.6902604182061),.UNSPECIFIED.);
#394=B_SPLINE_CURVE_WITH_KNOTS('',3,(#8820,#8821,#8822,#8823,#8824,#8825,
#8826,#8827,#8828,#8829),.UNSPECIFIED.,.F.,.F.,(4,1,1,1,1,1,1,4),(53.4070751110265,
54.3053527207099,55.3030265355533,56.3007003503968,57.2983741652402,58.2960479800837,
59.2937217949271,59.6902604182061),.UNSPECIFIED.);
#395=B_SPLINE_CURVE_WITH_KNOTS('',3,(#8834,#8835,#8836,#8837,#8838,#8839,
#8840,#8841,#8842,#8843),.UNSPECIFIED.,.F.,.F.,(4,1,1,1,1,1,1,4),(47.1238898038469,
47.775246196672,48.7729200115155,49.7705938263589,50.7682676412024,51.7659414560458,
52.7636152708893,53.4070751110265),.UNSPECIFIED.);
#396=B_SPLINE_CURVE_WITH_KNOTS('',3,(#8844,#8845,#8846,#8847,#8848,#8849,
#8850,#8851,#8852,#8853,#8854),.UNSPECIFIED.,.F.,.F.,(4,1,1,1,1,1,1,1,4),
(47.1238898038469,47.3216360168057,48.3193098316492,49.3169836464926,50.3146574613361,
51.3123312761795,52.310005091023,53.3076789058664,53.4070751110265),
 .UNSPECIFIED.);
#397=B_SPLINE_CURVE_WITH_KNOTS('',3,(#8859,#8860,#8861,#8862,#8863,#8864,
#8865,#8866,#8867,#8868),.UNSPECIFIED.,.F.,.F.,(4,1,1,1,1,1,1,4),(40.8407044966673,
41.7892033076113,42.7868771224548,43.7845509372982,44.7822247521417,45.7798985669851,
46.7775723818286,47.1238898038469),.UNSPECIFIED.);
#398=B_SPLINE_CURVE_WITH_KNOTS('',3,(#8869,#8870,#8871,#8872,#8873,#8874,
#8875,#8876,#8877,#8878),.UNSPECIFIED.,.F.,.F.,(4,1,1,1,1,1,1,4),(40.8407044966673,
41.335593127745,42.3332669425885,43.3309407574319,44.3286145722754,45.3262883871188,
46.3239622019623,47.1238898038469),.UNSPECIFIED.);
#399=B_SPLINE_CURVE_WITH_KNOTS('',3,(#8883,#8884,#8885,#8886,#8887,#8888,
#8889,#8890,#8891,#8892,#8893),.UNSPECIFIED.,.F.,.F.,(4,1,1,1,1,1,1,1,4),
(34.5575191894877,34.8054866037072,35.8031604185506,36.8008342333941,37.7985080482375,
38.796181863081,39.7938556779244,40.7915294927679,40.8407044966673),
 .UNSPECIFIED.);
#400=B_SPLINE_CURVE_WITH_KNOTS('',3,(#8894,#8895,#8896,#8897,#8898,#8899,
#8900,#8901,#8902,#8903),.UNSPECIFIED.,.F.,.F.,(4,1,1,1,1,1,1,4),(34.5575191894877,
35.3495502386843,36.3472240535278,37.3448978683712,38.3425716832147,39.3402454980581,
40.3379193129016,40.8407044966673),.UNSPECIFIED.);
#401=B_SPLINE_CURVE_WITH_KNOTS('',3,(#8908,#8909,#8910,#8911,#8912,#8913,
#8914,#8915,#8916,#8917),.UNSPECIFIED.,.F.,.F.,(4,1,1,1,1,1,1,4),(28.2743338823081,
28.8194437146465,29.8171175294899,30.8147913443334,31.8124651591768,32.8101389740203,
33.8078127888637,34.5575191894877),.UNSPECIFIED.);
#402=B_SPLINE_CURVE_WITH_KNOTS('',3,(#8918,#8919,#8920,#8921,#8922,#8923,
#8924,#8925,#8926,#8927,#8928),.UNSPECIFIED.,.F.,.F.,(4,1,1,1,1,1,1,1,4),
(28.2743338823081,28.3658335347801,29.3635073496236,30.361181164467,31.3588549793105,
32.3565287941539,33.3542026089974,34.3518764238408,34.5575191894877),
 .UNSPECIFIED.);
#403=B_SPLINE_CURVE_WITH_KNOTS('',3,(#8933,#8934,#8935,#8936,#8937,#8938,
#8939,#8940,#8941,#8942),.UNSPECIFIED.,.F.,.F.,(4,1,1,1,1,1,1,4),(21.9911485751285,
22.8334008255858,23.8310746404292,24.8287484552727,25.8264222701161,26.8240960849596,
27.821769899803,28.2743338823081),.UNSPECIFIED.);
#404=B_SPLINE_CURVE_WITH_KNOTS('',3,(#8943,#8944,#8945,#8946,#8947,#8948,
#8949,#8950,#8951,#8952),.UNSPECIFIED.,.F.,.F.,(4,1,1,1,1,1,1,4),(21.9911485751285,
22.3797906457194,23.3774644605629,24.3751382754063,25.3728120902498,26.3704859050932,
27.3681597199367,28.2743338823081),.UNSPECIFIED.);
#405=B_SPLINE_CURVE_WITH_KNOTS('',3,(#8958,#8959,#8960,#8961,#8962),
 .UNSPECIFIED.,.F.,.F.,(4,1,4),(14.3984001269718,15.3960739418153,15.7079632679489),
 .UNSPECIFIED.);
#406=B_SPLINE_CURVE_WITH_KNOTS('',3,(#8965,#8966,#8967,#8968,#8969),
 .UNSPECIFIED.,.F.,.F.,(4,1,4),(13.8759337553362,14.8520103068381,15.7079632679489),
 .UNSPECIFIED.);
#407=B_SPLINE_CURVE_WITH_KNOTS('',3,(#8971,#8972,#8973,#8974,#8975,#8976,
#8977,#8978,#8979,#8980,#8981),.UNSPECIFIED.,.F.,.F.,(4,1,1,1,1,1,1,1,4),
(15.7079632679489,15.8496841216816,16.8473579365251,17.8450317513685,18.842705566212,
19.8403793810554,20.8380531958989,21.8357270107423,21.9911485751285),
 .UNSPECIFIED.);
#408=B_SPLINE_CURVE_WITH_KNOTS('',3,(#8982,#8983,#8984,#8985,#8986,#8987,
#8988,#8989,#8990,#8991),.UNSPECIFIED.,.F.,.F.,(4,1,1,1,1,1,1,4),(15.7079632679489,
16.3937477566587,17.3914215715022,18.3890953863456,19.3867692011891,20.3844430160325,
21.382116830876,21.9911485751285),.UNSPECIFIED.);
#409=B_SPLINE_CURVE_WITH_KNOTS('',3,(#9264,#9265,#9266,#9267,#9268,#9269,
#9270,#9271,#9272,#9273,#9274,#9275,#9276,#9277,#9278,#9279,#9280,#9281,
#9282,#9283,#9284,#9285,#9286,#9287,#9288,#9289,#9290,#9291,#9292,#9293,
#9294,#9295,#9296,#9297,#9298,#9299,#9300,#9301,#9302,#9303,#9304,#9305,
#9306,#9307,#9308,#9309,#9310,#9311,#9312,#9313,#9314,#9315,#9316,#9317,
#9318,#9319,#9320,#9321,#9322,#9323,#9324,#9325,#9326,#9327,#9328,#9329,
#9330,#9331,#9332,#9333,#9334,#9335,#9336,#9337,#9338,#9339,#9340,#9341,
#9342,#9343,#9344,#9345,#9346,#9347,#9348,#9349,#9350,#9351,#9352,#9353,
#9354,#9355,#9356,#9357),.UNSPECIFIED.,.F.,.F.,(4,3,3,3,3,3,3,3,3,3,3,3,
3,3,3,3,3,3,3,3,3,3,3,3,3,3,3,3,3,3,3,4),(0.,0.0297253856296242,0.0601108027378182,
0.0895285923314871,0.115269158225947,0.120663203154239,0.150426123645478,
0.180024242366161,0.208881461646413,0.221328534043225,0.230191839641767,
0.234061656880844,0.262605657052961,0.290518670715962,0.295453119487169,
0.324405064850195,0.334115170721295,0.339546989903195,0.343311812224126,
0.371402280037358,0.399548859805574,0.427297746231078,0.438086546423522,
0.4438564739476,0.448937779695101,0.477641116182565,0.499168618548163,0.50804276641633,
0.513343558540668,0.539242379724507,0.563751125644957,0.569248610399426),
 .UNSPECIFIED.);
#410=B_SPLINE_CURVE_WITH_KNOTS('',3,(#9358,#9359,#9360,#9361,#9362,#9363,
#9364,#9365,#9366,#9367,#9368,#9369,#9370,#9371,#9372,#9373,#9374,#9375,
#9376,#9377,#9378,#9379,#9380,#9381,#9382,#9383,#9384,#9385,#9386,#9387,
#9388,#9389,#9390,#9391,#9392,#9393,#9394,#9395,#9396,#9397,#9398,#9399,
#9400,#9401,#9402,#9403,#9404,#9405,#9406,#9407,#9408,#9409,#9410,#9411,
#9412,#9413,#9414,#9415,#9416,#9417,#9418,#9419,#9420,#9421,#9422,#9423,
#9424,#9425,#9426,#9427,#9428,#9429,#9430,#9431,#9432,#9433,#9434,#9435,
#9436,#9437,#9438,#9439,#9440,#9441,#9442,#9443,#9444,#9445,#9446,#9447,
#9448,#9449,#9450,#9451,#9452,#9453,#9454),.UNSPECIFIED.,.F.,.F.,(4,3,3,
3,3,3,3,3,3,3,3,3,3,3,3,3,3,3,3,3,3,3,3,3,3,3,3,3,3,3,3,3,4),(0.,0.0253648787438216,
0.0514012503296148,0.0783340991562622,0.0901172205179204,0.0965533763871403,
0.102698976537763,0.130004344707653,0.157760279045425,0.185036219519768,
0.195822086385967,0.202205933167581,0.206455228577107,0.235058197592291,
0.263563073600605,0.266864040942794,0.294771372010393,0.305811990557415,
0.311201564685129,0.315692000115899,0.343784542768854,0.372917960011625,
0.402371202344126,0.413838480330537,0.423017273727782,0.428134361040601,
0.458199607388461,0.483702640496826,0.492128633871143,0.498168341087558,
0.529190040454739,0.56021173982192,0.566847306048046),.UNSPECIFIED.);
#411=B_SPLINE_CURVE_WITH_KNOTS('',3,(#9455,#9456,#9457,#9458,#9459,#9460,
#9461,#9462,#9463,#9464,#9465,#9466,#9467,#9468,#9469,#9470,#9471,#9472,
#9473,#9474,#9475,#9476,#9477,#9478,#9479),.UNSPECIFIED.,.F.,.F.,(4,3,3,
3,3,3,3,3,4),(-10.1321597128207,-9.9767381484345,-8.97906433359106,-7.9813905187476,
-6.98371670390416,-5.9860428890607,-4.98836907421726,-3.9906952593738,-3.84897440564114),
 .UNSPECIFIED.);
#412=B_SPLINE_CURVE_WITH_KNOTS('',3,(#9752,#9753,#9754,#9755,#9756,#9757,
#9758,#9759,#9760,#9761,#9762,#9763,#9764,#9765,#9766,#9767,#9768,#9769,
#9770,#9771,#9772,#9773,#9774,#9775,#9776,#9777,#9778,#9779,#9780,#9781,
#9782,#9783,#9784,#9785,#9786,#9787,#9788,#9789,#9790,#9791,#9792,#9793,
#9794,#9795,#9796,#9797,#9798,#9799,#9800,#9801,#9802,#9803,#9804,#9805,
#9806,#9807,#9808,#9809,#9810,#9811,#9812,#9813,#9814,#9815,#9816,#9817,
#9818,#9819,#9820,#9821,#9822,#9823,#9824,#9825,#9826,#9827,#9828,#9829,
#9830,#9831,#9832,#9833,#9834,#9835,#9836,#9837,#9838,#9839,#9840,#9841,
#9842,#9843,#9844,#9845,#9846,#9847,#9848),.UNSPECIFIED.,.F.,.F.,(4,3,3,
3,3,3,3,3,3,3,3,3,3,3,3,3,3,3,3,3,3,3,3,3,3,3,3,3,3,3,3,3,4),(0.,0.0253648724852029,
0.0514012384230764,0.0783340887380444,0.0901172107508429,0.0965533720660576,
0.102698977879582,0.130004341727049,0.157760273968556,0.185036215712122,
0.195822085350035,0.202205931968829,0.206455227843058,0.235058195828899,
0.263563073798338,0.26686404094282,0.294771375027874,0.305811996926419,
0.311201630318074,0.31569201086916,0.343784558171023,0.372917977567861,
0.402371220433395,0.413838515963309,0.423017671022353,0.428134408783598,
0.458199656551482,0.483702677369108,0.492128800036471,0.498168345990172,
0.529190042906079,0.560211739821985,0.56684730604811),.UNSPECIFIED.);
#413=B_SPLINE_CURVE_WITH_KNOTS('',3,(#9849,#9850,#9851,#9852,#9853,#9854,
#9855,#9856,#9857,#9858,#9859,#9860,#9861,#9862,#9863,#9864,#9865,#9866,
#9867,#9868,#9869,#9870),.UNSPECIFIED.,.F.,.F.,(4,3,3,3,3,3,3,4),(7.59274844815666,
7.9813905187476,8.97906433359105,9.97673814843451,10.974411963278,11.9720857781214,
12.9697595929649,13.8759337553362),.UNSPECIFIED.);
#414=B_SPLINE_CURVE_WITH_KNOTS('',3,(#9871,#9872,#9873,#9874,#9875,#9876,
#9877,#9878,#9879,#9880,#9881,#9882,#9883,#9884,#9885,#9886,#9887,#9888,
#9889,#9890,#9891,#9892,#9893,#9894,#9895,#9896,#9897,#9898,#9899,#9900,
#9901,#9902,#9903,#9904,#9905,#9906,#9907,#9908,#9909,#9910,#9911,#9912,
#9913,#9914,#9915,#9916,#9917,#9918,#9919,#9920,#9921,#9922,#9923,#9924,
#9925,#9926,#9927,#9928,#9929,#9930,#9931,#9932,#9933,#9934,#9935,#9936,
#9937,#9938,#9939,#9940,#9941,#9942,#9943,#9944,#9945,#9946,#9947,#9948,
#9949,#9950,#9951,#9952,#9953,#9954,#9955,#9956,#9957,#9958,#9959,#9960,
#9961,#9962,#9963,#9964),.UNSPECIFIED.,.F.,.F.,(4,3,3,3,3,3,3,3,3,3,3,3,
3,3,3,3,3,3,3,3,3,3,3,3,3,3,3,3,3,3,3,4),(0.,0.0297253803932464,0.0601107949195137,
0.0895285854904694,0.115269152240056,0.120663201907019,0.150426122369489,
0.180024242551286,0.208881461785255,0.221328534890279,0.230191850972631,
0.234061673089794,0.262605674713976,0.290518689511932,0.295453119487159,
0.324405064607358,0.334115171284016,0.339546990350236,0.343311812881693,
0.371402280552886,0.399548860319871,0.427297747957366,0.43808655063386,
0.443856478069222,0.448937779896069,0.477641116333293,0.499168618661212,
0.508042768434368,0.513343559316224,0.53924238350147,0.563751125644968,
0.569248610399442),.UNSPECIFIED.);
#415=B_SPLINE_CURVE_WITH_KNOTS('',3,(#9974,#9975,#9976,#9977,#9978,#9979,
#9980,#9981,#9982,#9983,#9984,#9985,#9986,#9987,#9988,#9989,#9990,#9991,
#9992,#9993,#9994,#9995,#9996,#9997,#9998,#9999,#10000,#10001,#10002,#10003,
#10004,#10005,#10006,#10007,#10008,#10009,#10010,#10011,#10012,#10013,#10014,
#10015,#10016,#10017,#10018,#10019,#10020,#10021,#10022,#10023,#10024,#10025,
#10026,#10027,#10028,#10029,#10030,#10031,#10032,#10033,#10034,#10035,#10036,
#10037,#10038,#10039,#10040,#10041,#10042,#10043,#10044,#10045,#10046,#10047,
#10048,#10049,#10050,#10051,#10052,#10053,#10054,#10055,#10056,#10057,#10058,
#10059,#10060,#10061,#10062,#10063,#10064,#10065,#10066,#10067,#10068,#10069,
#10070),.UNSPECIFIED.,.F.,.F.,(4,3,3,3,3,3,3,3,3,3,3,3,3,3,3,3,3,3,3,3,
3,3,3,3,3,3,3,3,3,3,3,3,4),(0.,0.0253648605053273,0.0514012156305792,0.0783340687946069,
0.0901171920538689,0.0965533637916206,0.102698980421147,0.130004335995597,
0.157760264221757,0.185036208402018,0.195822083362881,0.202205929681762,
0.206455226436585,0.235058192455082,0.263563074173201,0.2668640409428,0.294771380802971,
0.305812009113333,0.311201755151532,0.315692031327867,0.343784587536137,
0.372918011054392,0.402371254938888,0.413838583941099,0.4230184291352,0.428134500012189,
0.458199750478009,0.483702747813993,0.492129117528397,0.498168355355325,
0.529190047588635,0.560211739821945,0.566847306048074),.UNSPECIFIED.);
#416=B_SPLINE_CURVE_WITH_KNOTS('',3,(#10071,#10072,#10073,#10074,#10075,
#10076,#10077,#10078,#10079,#10080,#10081,#10082,#10083,#10084,#10085,#10086,
#10087,#10088,#10089,#10090,#10091,#10092,#10093,#10094,#10095,#10096,#10097,
#10098,#10099,#10100,#10101,#10102,#10103,#10104,#10105,#10106,#10107,#10108,
#10109,#10110,#10111,#10112,#10113,#10114,#10115,#10116,#10117,#10118,#10119,
#10120,#10121,#10122,#10123,#10124,#10125,#10126,#10127,#10128,#10129,#10130,
#10131,#10132,#10133,#10134,#10135,#10136,#10137,#10138,#10139,#10140,#10141,
#10142,#10143,#10144,#10145,#10146,#10147,#10148,#10149,#10150,#10151,#10152,
#10153,#10154,#10155,#10156,#10157,#10158,#10159,#10160,#10161,#10162,#10163,
#10164),.UNSPECIFIED.,.F.,.F.,(4,3,3,3,3,3,3,3,3,3,3,3,3,3,3,3,3,3,3,3,
3,3,3,3,3,3,3,3,3,3,3,4),(0.,0.0297254323827744,0.0601108725400646,0.0895286534084515,
0.11526921166829,0.12066321428879,0.150426135046203,0.180024240717284,0.208881460409753,
0.221328526477776,0.230191738437716,0.234061511334529,0.262605498546548,
0.290518502067642,0.29545311948716,0.324405067020953,0.334115165693271,
0.339546985526679,0.343311805029728,0.371402274101902,0.399548853885078,
0.42729772947452,0.438086506007797,0.443856434974185,0.44893777735014,0.477641114423841,
0.499168617229116,0.508042746133096,0.513343551251566,0.539242345608596,
0.563751125644942,0.569248610399418),.UNSPECIFIED.);
#417=B_SPLINE_CURVE_WITH_KNOTS('',3,(#10165,#10166,#10167,#10168,#10169,
#10170,#10171,#10172,#10173,#10174,#10175,#10176,#10177,#10178,#10179,#10180,
#10181,#10182,#10183,#10184,#10185,#10186,#10187,#10188,#10189,#10190,#10191,
#10192,#10193,#10194,#10195,#10196,#10197,#10198,#10199,#10200,#10201,#10202,
#10203,#10204,#10205,#10206,#10207,#10208,#10209,#10210,#10211,#10212,#10213,
#10214,#10215,#10216,#10217,#10218,#10219,#10220,#10221,#10222,#10223,#10224,
#10225,#10226,#10227,#10228,#10229,#10230,#10231,#10232,#10233,#10234,#10235,
#10236,#10237,#10238,#10239,#10240,#10241,#10242,#10243,#10244,#10245,#10246,
#10247,#10248,#10249,#10250,#10251,#10252,#10253,#10254,#10255,#10256,#10257,
#10258,#10259,#10260,#10261),.UNSPECIFIED.,.F.,.F.,(4,3,3,3,3,3,3,3,3,3,
3,3,3,3,3,3,3,3,3,3,3,3,3,3,3,3,3,3,3,3,3,3,4),(0.,0.0253648987606154,0.0514012884108024,
0.0783341324773016,0.0901172517563951,0.0965533902110582,0.102698972275023,
0.130004354267608,0.157760295311984,0.185036231719687,0.195822089703329,
0.202205936992556,0.206455230916444,0.235058203214103,0.263563072953794,
0.266864040942797,0.294771362359164,0.305811970189412,0.311201355676537,
0.315691965877597,0.343784493654311,0.372917904009451,0.402371144638991,
0.413838366652747,0.423016006622453,0.42813420907177,0.458199450904524,
0.483702523133876,0.492128105008987,0.498168325925378,0.529190032873656,
0.560211739821933,0.566847306048061),.UNSPECIFIED.);
#418=B_SPLINE_CURVE_WITH_KNOTS('',3,(#10262,#10263,#10264,#10265,#10266,
#10267,#10268,#10269,#10270,#10271,#10272,#10273,#10274,#10275,#10276,#10277,
#10278,#10279,#10280,#10281,#10282,#10283,#10284,#10285,#10286,#10287,#10288,
#10289,#10290,#10291,#10292,#10293,#10294,#10295,#10296,#10297,#10298,#10299,
#10300,#10301,#10302,#10303,#10304,#10305,#10306,#10307,#10308,#10309,#10310,
#10311,#10312,#10313,#10314,#10315,#10316,#10317,#10318,#10319,#10320,#10321,
#10322,#10323,#10324,#10325,#10326,#10327,#10328,#10329,#10330,#10331,#10332,
#10333,#10334,#10335,#10336,#10337,#10338,#10339,#10340,#10341,#10342,#10343,
#10344,#10345,#10346,#10347,#10348,#10349,#10350,#10351,#10352,#10353,#10354,
#10355),.UNSPECIFIED.,.F.,.F.,(4,3,3,3,3,3,3,3,3,3,3,3,3,3,3,3,3,3,3,3,
3,3,3,3,3,3,3,3,3,3,3,4),(0.,0.0297253962397254,0.0601108185791267,0.0895286061926336,
0.115269170354452,0.12066320568266,0.150426126236148,0.180024241996468,
0.208881461369146,0.221328532330586,0.230191816729447,0.23406162386096,
0.262605621092836,0.290518632453638,0.295453119487182,0.324405065342412,
0.334115169579262,0.339546988882028,0.343311810500951,0.371402278599766,
0.399548858373274,0.427297742341304,0.438086537068835,0.443856464964634,
0.448937779125463,0.477641115755344,0.499168618227755,0.508042761654416,
0.513343556861467,0.539242371960185,0.563751125644987,0.569248610399463),
 .UNSPECIFIED.);
#419=B_SPLINE_CURVE_WITH_KNOTS('',3,(#10356,#10357,#10358,#10359,#10360,
#10361,#10362,#10363,#10364,#10365,#10366,#10367,#10368,#10369,#10370,#10371,
#10372,#10373,#10374,#10375,#10376,#10377,#10378,#10379,#10380,#10381,#10382,
#10383,#10384,#10385,#10386,#10387,#10388,#10389,#10390,#10391,#10392,#10393,
#10394,#10395,#10396,#10397,#10398,#10399,#10400,#10401,#10402,#10403,#10404,
#10405,#10406,#10407,#10408,#10409,#10410,#10411,#10412,#10413,#10414,#10415,
#10416,#10417,#10418,#10419,#10420,#10421,#10422,#10423,#10424,#10425,#10426,
#10427,#10428,#10429,#10430,#10431,#10432,#10433,#10434,#10435,#10436,#10437,
#10438,#10439,#10440,#10441,#10442,#10443,#10444,#10445,#10446,#10447,#10448,
#10449,#10450,#10451,#10452),.UNSPECIFIED.,.F.,.F.,(4,3,3,3,3,3,3,3,3,3,
3,3,3,3,3,3,3,3,3,3,3,3,3,3,3,3,3,3,3,3,3,3,4),(0.,0.025364844042126,0.0514011843088595,
0.0783340413881027,0.0901171663602716,0.0965533524230185,0.102698983918303,
0.130004328122858,0.157760250831759,0.185036198359521,0.195822080632133,
0.20220592653402,0.206455224516067,0.235058187831454,0.263563074702486,
0.266864040942805,0.294771388738814,0.30581202586054,0.311201927094549,
0.315692059513443,0.343784627954795,0.372918057137183,0.402371302422366,
0.413838677482968,0.423019472683294,0.428134625857437,0.458199880044474,
0.483702844988851,0.492129555524298,0.498168368529568,0.529190054175775,
0.560211739821982,0.566847306048111),.UNSPECIFIED.);
#420=B_SPLINE_CURVE_WITH_KNOTS('',3,(#10453,#10454,#10455,#10456,#10457,
#10458,#10459,#10460,#10461,#10462,#10463,#10464,#10465,#10466,#10467,#10468,
#10469,#10470,#10471,#10472,#10473,#10474,#10475,#10476,#10477,#10478,#10479,
#10480,#10481,#10482,#10483,#10484,#10485,#10486,#10487,#10488,#10489,#10490,
#10491,#10492,#10493,#10494,#10495,#10496,#10497,#10498,#10499,#10500,#10501,
#10502,#10503,#10504,#10505,#10506,#10507,#10508,#10509,#10510,#10511,#10512,
#10513,#10514,#10515,#10516,#10517,#10518,#10519,#10520,#10521,#10522,#10523,
#10524,#10525,#10526,#10527,#10528,#10529,#10530,#10531,#10532,#10533,#10534,
#10535,#10536,#10537,#10538,#10539,#10540,#10541,#10542,#10543,#10544,#10545,
#10546),.UNSPECIFIED.,.F.,.F.,(4,3,3,3,3,3,3,3,3,3,3,3,3,3,3,3,3,3,3,3,
3,3,3,3,3,3,3,3,3,3,3,4),(0.,0.0297254135725658,0.0601108444573347,0.0895286288360644,
0.115269190167453,0.120663209818937,0.15042613047052,0.180024241393071,
0.208881460916596,0.221328529533058,0.230191779298948,0.234061570055621,
0.262605562480418,0.290518570080715,0.295453119487172,0.324405066148158,
0.334115167717825,0.339546987280336,0.343311807892538,0.371402276458584,
0.399548856237476,0.42729773618933,0.438086522212006,0.443856450609684,
0.448937778272206,0.477641115115396,0.499168617747789,0.508042754204043,
0.513343554169974,0.539242359324933,0.563751125644967,0.569248610399445),
 .UNSPECIFIED.);
#421=B_SPLINE_CURVE_WITH_KNOTS('',3,(#10548,#10549,#10550,#10551,#10552,
#10553,#10554,#10555,#10556,#10557,#10558),.UNSPECIFIED.,.F.,.F.,(4,1,1,
1,1,1,1,1,4),(15.7079632679489,15.8496841216816,16.847357936525,17.8450317513685,
18.8427055662119,19.8403793810554,20.8380531958989,21.8357270107423,21.9911485751285),
 .UNSPECIFIED.);
#422=B_SPLINE_CURVE_WITH_KNOTS('',3,(#10559,#10560,#10561,#10562,#10563,
#10564,#10565,#10566,#10567,#10568),.UNSPECIFIED.,.F.,.F.,(4,1,1,1,1,1,
1,4),(15.7079632679489,16.3937477566587,17.3914215715022,18.3890953863456,
19.3867692011891,20.3844430160325,21.382116830876,21.9911485751285),
 .UNSPECIFIED.);
#423=B_SPLINE_CURVE_WITH_KNOTS('',3,(#10841,#10842,#10843,#10844,#10845,
#10846,#10847,#10848,#10849,#10850,#10851,#10852,#10853,#10854,#10855,#10856,
#10857,#10858,#10859,#10860,#10861,#10862,#10863,#10864,#10865,#10866,#10867,
#10868,#10869,#10870,#10871,#10872,#10873,#10874,#10875,#10876,#10877,#10878,
#10879,#10880,#10881,#10882,#10883,#10884,#10885,#10886,#10887,#10888,#10889,
#10890,#10891,#10892,#10893,#10894,#10895,#10896,#10897,#10898,#10899,#10900,
#10901,#10902,#10903,#10904,#10905,#10906,#10907,#10908,#10909,#10910,#10911,
#10912,#10913,#10914,#10915,#10916,#10917,#10918,#10919,#10920,#10921,#10922,
#10923,#10924,#10925,#10926,#10927,#10928,#10929,#10930,#10931,#10932,#10933,
#10934),.UNSPECIFIED.,.F.,.F.,(4,3,3,3,3,3,3,3,3,3,3,3,3,3,3,3,3,3,3,3,
3,3,3,3,3,3,3,3,3,3,3,4),(0.,0.0297253703679347,0.0601107799498536,0.0895285723920194,
0.115269140778915,0.120663199497391,0.150426119902105,0.180024242882666,
0.208881462033794,0.221328536492063,0.230191872423422,0.234061703914739,
0.262605708325631,0.290518725301924,0.29545311948718,0.32440506413479,0.334115172344466,
0.339546991246465,0.343311814329514,0.37140228172866,0.399548861491339,
0.427297751445956,0.438086559078568,0.443856486243239,0.448937780382051,
0.477641116697784,0.499168618934584,0.508042772723187,0.513343560868865,
0.539242390799467,0.563751125644983,0.569248610399456),.UNSPECIFIED.);
#424=B_SPLINE_CURVE_WITH_KNOTS('',3,(#10935,#10936,#10937,#10938,#10939,
#10940,#10941,#10942,#10943,#10944,#10945,#10946,#10947,#10948,#10949,#10950,
#10951,#10952,#10953,#10954,#10955,#10956,#10957,#10958,#10959),
 .UNSPECIFIED.,.F.,.F.,(4,3,3,3,3,3,3,3,4),(-10.1321597128207,-9.97673814843451,
-8.97906433359106,-7.98139051874761,-6.98371670390416,-5.98604288906071,
-4.98836907421726,-3.9906952593738,-3.84897440564114),.UNSPECIFIED.);
#425=B_SPLINE_CURVE_WITH_KNOTS('',3,(#11232,#11233,#11234,#11235,#11236,
#11237,#11238,#11239,#11240,#11241,#11242,#11243,#11244,#11245,#11246,#11247,
#11248,#11249,#11250,#11251,#11252,#11253,#11254,#11255,#11256,#11257,#11258,
#11259,#11260,#11261,#11262,#11263,#11264,#11265,#11266,#11267,#11268,#11269,
#11270,#11271,#11272,#11273,#11274,#11275,#11276,#11277,#11278,#11279,#11280,
#11281,#11282,#11283,#11284,#11285,#11286,#11287,#11288,#11289,#11290,#11291,
#11292,#11293,#11294,#11295,#11296,#11297,#11298,#11299,#11300,#11301,#11302,
#11303,#11304,#11305,#11306,#11307,#11308,#11309,#11310,#11311,#11312,#11313,
#11314,#11315,#11316,#11317,#11318,#11319,#11320,#11321,#11322,#11323,#11324,
#11325,#11326,#11327,#11328),.UNSPECIFIED.,.F.,.F.,(4,3,3,3,3,3,3,3,3,3,
3,3,3,3,3,3,3,3,3,3,3,3,3,3,3,3,3,3,3,3,3,3,4),(0.,0.0253649346248504,0.0514013566484054,
0.0783341921852065,0.090117307732557,0.0965534149831339,0.102698964686601,
0.130004371440625,0.157760324498296,0.185036253609426,0.195822095654156,
0.202205943841528,0.2064552351094,0.235058213296301,0.263563071795369,0.266864040942814,
0.294771345060892,0.305811933683324,0.311200980890666,0.315691904514554,
0.343784405626614,0.372917803637586,0.402371041212361,0.413838162909138,
0.423013737084902,0.428133938024777,0.458199171791025,0.483702313798766,
0.492127161867958,0.498168299793874,0.529190019807931,0.560211739821988,
0.566847306048107),.UNSPECIFIED.);
#426=B_SPLINE_CURVE_WITH_KNOTS('',3,(#11329,#11330,#11331,#11332,#11333,
#11334,#11335,#11336,#11337,#11338,#11339,#11340,#11341,#11342,#11343,#11344,
#11345,#11346,#11347,#11348,#11349,#11350),.UNSPECIFIED.,.F.,.F.,(4,3,3,
3,3,3,3,4),(7.59274844815666,7.98139051874761,8.97906433359106,9.97673814843451,
10.974411963278,11.9720857781214,12.9697595929649,13.8759337553362),
 .UNSPECIFIED.);
#427=B_SPLINE_CURVE_WITH_KNOTS('',3,(#11352,#11353,#11354,#11355,#11356,
#11357,#11358,#11359,#11360,#11361,#11362),.UNSPECIFIED.,.F.,.F.,(4,1,1,
1,1,1,1,1,4),(15.7079632679489,15.8496841216816,16.847357936525,17.8450317513685,
18.8427055662119,19.8403793810554,20.8380531958988,21.8357270107423,21.9911485751285),
 .UNSPECIFIED.);
#428=B_SPLINE_CURVE_WITH_KNOTS('',3,(#11363,#11364,#11365,#11366,#11367,
#11368,#11369,#11370,#11371,#11372),.UNSPECIFIED.,.F.,.F.,(4,1,1,1,1,1,
1,4),(15.7079632679489,16.3937477566587,17.3914215715022,18.3890953863456,
19.3867692011891,20.3844430160325,21.382116830876,21.9911485751285),
 .UNSPECIFIED.);
#429=B_SPLINE_CURVE_WITH_KNOTS('',3,(#11645,#11646,#11647,#11648,#11649,
#11650,#11651,#11652,#11653,#11654,#11655,#11656,#11657,#11658,#11659,#11660,
#11661,#11662,#11663,#11664,#11665,#11666,#11667,#11668,#11669,#11670,#11671,
#11672,#11673,#11674,#11675,#11676,#11677,#11678,#11679,#11680,#11681,#11682,
#11683,#11684,#11685,#11686,#11687,#11688,#11689,#11690,#11691,#11692,#11693,
#11694,#11695,#11696,#11697,#11698,#11699,#11700,#11701,#11702,#11703,#11704,
#11705,#11706,#11707,#11708,#11709,#11710,#11711,#11712,#11713,#11714,#11715,
#11716,#11717,#11718,#11719,#11720,#11721,#11722,#11723,#11724,#11725,#11726,
#11727,#11728,#11729,#11730,#11731,#11732,#11733,#11734,#11735,#11736,#11737,
#11738),.UNSPECIFIED.,.F.,.F.,(4,3,3,3,3,3,3,3,3,3,3,3,3,3,3,3,3,3,3,3,
3,3,3,3,3,3,3,3,3,3,3,4),(0.,0.0297254023740782,0.0601108277330677,0.0895286142023326,
0.115269177362939,0.120663207133914,0.15042612772287,0.180024241772488,
0.208881461201163,0.221328531331202,0.230191803363959,0.234061604650791,
0.262605600181984,0.290518610215652,0.295453119487186,0.324405065627094,
0.334115168920554,0.339546988327522,0.343311809571304,0.371402277835618,
0.399548857610104,0.427297740159933,0.438086531802328,0.443856459882809,
0.448937778846684,0.477641115546252,0.499168618070928,0.508042759111529,
0.513343555924621,0.539242367504077,0.563751125644955,0.569248610399431),
 .UNSPECIFIED.);
#430=B_SPLINE_CURVE_WITH_KNOTS('',3,(#11739,#11740,#11741,#11742,#11743,
#11744,#11745,#11746,#11747,#11748,#11749,#11750,#11751,#11752,#11753,#11754,
#11755,#11756,#11757,#11758,#11759,#11760,#11761,#11762,#11763),
 .UNSPECIFIED.,.F.,.F.,(4,3,3,3,3,3,3,3,4),(-10.1321597128207,-9.97673814843451,
-8.97906433359106,-7.9813905187476,-6.98371670390416,-5.98604288906071,
-4.98836907421726,-3.99069525937381,-3.84897440564115),.UNSPECIFIED.);
#431=B_SPLINE_CURVE_WITH_KNOTS('',3,(#12036,#12037,#12038,#12039,#12040,
#12041,#12042,#12043,#12044,#12045,#12046,#12047,#12048,#12049,#12050,#12051,
#12052,#12053,#12054,#12055,#12056,#12057,#12058,#12059,#12060,#12061,#12062,
#12063,#12064,#12065,#12066,#12067,#12068,#12069,#12070,#12071,#12072,#12073,
#12074,#12075,#12076,#12077,#12078,#12079,#12080,#12081,#12082,#12083,#12084,
#12085,#12086,#12087,#12088,#12089,#12090,#12091,#12092,#12093,#12094,#12095,
#12096,#12097,#12098,#12099,#12100,#12101,#12102,#12103,#12104,#12105,#12106,
#12107,#12108,#12109,#12110,#12111,#12112,#12113,#12114,#12115,#12116,#12117,
#12118,#12119,#12120,#12121,#12122,#12123,#12124,#12125,#12126,#12127,#12128,
#12129,#12130,#12131,#12132),.UNSPECIFIED.,.F.,.F.,(4,3,3,3,3,3,3,3,3,3,
3,3,3,3,3,3,3,3,3,3,3,3,3,3,3,3,3,3,3,3,3,3,4),(0.,0.0253648914275516,0.0514012744616646,
0.078334120271809,0.0901172403137471,0.0965533851472873,0.102698973861186,
0.130004350789599,0.157760289377991,0.185036227269198,0.195822088492465,
0.202205935589398,0.206455229962407,0.235058201053358,0.263563073088682,
0.26686404094282,0.294771365897737,0.305811977656062,0.311201432434786,
0.315691978449507,0.343784511677691,0.37291792455713,0.402371165813427,
0.413838408362615,0.423016471455126,0.42813426476668,0.458199508244744,
0.483702566139053,0.492128298799099,0.49816833135269,0.529190035587335,
0.560211739821979,0.566847306048113),.UNSPECIFIED.);
#432=B_SPLINE_CURVE_WITH_KNOTS('',3,(#12133,#12134,#12135,#12136,#12137,
#12138,#12139,#12140,#12141,#12142,#12143,#12144,#12145,#12146,#12147,#12148,
#12149,#12150,#12151,#12152,#12153,#12154),.UNSPECIFIED.,.F.,.F.,(4,3,3,
3,3,3,3,4),(7.59274844815666,7.98139051874761,8.97906433359107,9.97673814843452,
10.974411963278,11.9720857781214,12.9697595929649,13.8759337553362),
 .UNSPECIFIED.);
#433=B_SPLINE_CURVE_WITH_KNOTS('',3,(#12156,#12157,#12158,#12159,#12160,
#12161,#12162,#12163,#12164,#12165,#12166),.UNSPECIFIED.,.F.,.F.,(4,1,1,
1,1,1,1,1,4),(15.7079632679489,15.8496841216816,16.8473579365251,17.8450317513685,
18.842705566212,19.8403793810554,20.8380531958989,21.8357270107423,21.9911485751285),
 .UNSPECIFIED.);
#434=B_SPLINE_CURVE_WITH_KNOTS('',3,(#12167,#12168,#12169,#12170,#12171,
#12172,#12173,#12174,#12175,#12176),.UNSPECIFIED.,.F.,.F.,(4,1,1,1,1,1,
1,4),(15.7079632679489,16.3937477566587,17.3914215715022,18.3890953863456,
19.3867692011891,20.3844430160325,21.382116830876,21.9911485751285),
 .UNSPECIFIED.);
#435=B_SPLINE_CURVE_WITH_KNOTS('',3,(#12449,#12450,#12451,#12452,#12453,
#12454,#12455,#12456,#12457,#12458,#12459,#12460,#12461,#12462,#12463,#12464,
#12465,#12466,#12467,#12468,#12469,#12470,#12471,#12472,#12473,#12474,#12475,
#12476,#12477,#12478,#12479,#12480,#12481,#12482,#12483,#12484,#12485,#12486,
#12487,#12488,#12489,#12490,#12491,#12492,#12493,#12494,#12495,#12496,#12497,
#12498,#12499,#12500,#12501,#12502,#12503,#12504,#12505,#12506,#12507,#12508,
#12509,#12510,#12511,#12512,#12513,#12514,#12515,#12516,#12517,#12518,#12519,
#12520,#12521,#12522,#12523,#12524,#12525,#12526,#12527,#12528,#12529,#12530,
#12531,#12532,#12533,#12534,#12535,#12536,#12537,#12538,#12539,#12540,#12541,
#12542),.UNSPECIFIED.,.F.,.F.,(4,3,3,3,3,3,3,3,3,3,3,3,3,3,3,3,3,3,3,3,
3,3,3,3,3,3,3,3,3,3,3,4),(0.,0.029725356595138,0.0601107593868406,0.0895285543993829,
0.115269125035357,0.12066319618678,0.150426116509258,0.180024243330567,
0.20888146236972,0.221328538686106,0.230191901801689,0.234061746102067,
0.262605754332067,0.290518774304223,0.295453119487179,0.324405063500147,
0.334115173835696,0.339546992466191,0.343311816416088,0.37140228344413,
0.399548863199563,0.427297756337497,0.438086570890066,0.443856497633085,
0.448937781098459,0.477641117235086,0.499168619337557,0.508042778795357,
0.513343563033152,0.539242400853845,0.563751125644967,0.569248610399444),
 .UNSPECIFIED.);
#436=B_SPLINE_CURVE_WITH_KNOTS('',3,(#12543,#12544,#12545,#12546,#12547,
#12548,#12549,#12550,#12551,#12552,#12553,#12554,#12555,#12556,#12557,#12558,
#12559,#12560,#12561,#12562,#12563,#12564,#12565,#12566,#12567),
 .UNSPECIFIED.,.F.,.F.,(4,3,3,3,3,3,3,3,4),(-10.1321597128207,-9.97673814843451,
-8.97906433359106,-7.98139051874761,-6.98371670390416,-5.98604288906071,
-4.98836907421726,-3.99069525937381,-3.84897440564113),.UNSPECIFIED.);
#437=B_SPLINE_CURVE_WITH_KNOTS('',3,(#12840,#12841,#12842,#12843,#12844,
#12845,#12846,#12847,#12848,#12849,#12850,#12851,#12852,#12853,#12854,#12855,
#12856,#12857,#12858,#12859,#12860,#12861,#12862,#12863,#12864,#12865,#12866,
#12867,#12868,#12869,#12870,#12871,#12872,#12873,#12874,#12875,#12876,#12877,
#12878,#12879,#12880,#12881,#12882,#12883,#12884,#12885,#12886,#12887,#12888,
#12889,#12890,#12891,#12892,#12893,#12894,#12895,#12896,#12897,#12898,#12899,
#12900,#12901,#12902,#12903,#12904,#12905,#12906,#12907,#12908,#12909,#12910,
#12911,#12912,#12913,#12914,#12915,#12916,#12917,#12918,#12919,#12920,#12921,
#12922,#12923,#12924,#12925,#12926,#12927,#12928,#12929,#12930,#12931,#12932,
#12933,#12934,#12935,#12936),.UNSPECIFIED.,.F.,.F.,(4,3,3,3,3,3,3,3,3,3,
3,3,3,3,3,3,3,3,3,3,3,3,3,3,3,3,3,3,3,3,3,3,4),(0.,0.0253649121453671,0.0514013138739685,
0.0783341547575759,0.0901172726441542,0.0965533994556431,0.102698969500997,
0.130004360735148,0.157760306262492,0.185036239932576,0.195822091936498,
0.202205939549384,0.206455232492389,0.235058206978254,0.263563072530515,
0.266864040942828,0.294771355900332,0.305811956558916,0.311201215703461,
0.315691942956057,0.343784460775633,0.372917866524038,0.40237110601464,
0.413838290565183,0.423015158860743,0.42813410765337,0.458199346461555,
0.48370244480167,0.492127752073996,0.498168316004108,0.529190027913061,
0.560211739822014,0.566847306048133),.UNSPECIFIED.);
#438=B_SPLINE_CURVE_WITH_KNOTS('',3,(#12937,#12938,#12939,#12940,#12941,
#12942,#12943,#12944,#12945,#12946,#12947,#12948,#12949,#12950,#12951,#12952,
#12953,#12954,#12955,#12956,#12957,#12958),.UNSPECIFIED.,.F.,.F.,(4,3,3,
3,3,3,3,4),(7.59274844815664,7.98139051874761,8.97906433359106,9.97673814843451,
10.974411963278,11.9720857781214,12.9697595929649,13.8759337553362),
 .UNSPECIFIED.);
#439=SHAPE_REPRESENTATION_RELATIONSHIP('SRR','None',#13328,#455);
#440=SHAPE_REPRESENTATION_RELATIONSHIP('SRR','None',#13329,#456);
#441=SHAPE_REPRESENTATION_RELATIONSHIP('SRR','None',#13330,#457);
#442=SHAPE_REPRESENTATION_RELATIONSHIP('SRR','None',#13331,#458);
#443=SHAPE_REPRESENTATION_RELATIONSHIP('SRR','None',#13332,#459);
#444=SHAPE_REPRESENTATION_RELATIONSHIP('SRR','None',#13333,#460);
#445=SHAPE_REPRESENTATION_RELATIONSHIP('SRR','None',#13334,#461);
#446=SHAPE_REPRESENTATION_RELATIONSHIP('SRR','None',#13335,#462);
#447=SHAPE_REPRESENTATION_RELATIONSHIP('SRR','None',#13336,#463);
#448=SHAPE_REPRESENTATION_RELATIONSHIP('SRR','None',#13337,#464);
#449=SHAPE_REPRESENTATION_RELATIONSHIP('SRR','None',#13338,#465);
#450=SHAPE_REPRESENTATION_RELATIONSHIP('SRR','None',#13339,#466);
#451=SHAPE_REPRESENTATION_RELATIONSHIP('SRR','None',#13340,#467);
#452=SHAPE_REPRESENTATION_RELATIONSHIP('SRR','None',#13341,#468);
#453=SHAPE_REPRESENTATION_RELATIONSHIP('SRR','None',#13342,#469);
#454=SHAPE_REPRESENTATION_RELATIONSHIP('SRR','None',#13343,#470);
#455=ADVANCED_BREP_SHAPE_REPRESENTATION('',(#487),#13215);
#456=ADVANCED_BREP_SHAPE_REPRESENTATION('',(#488),#13216);
#457=ADVANCED_BREP_SHAPE_REPRESENTATION('',(#489),#13217);
#458=ADVANCED_BREP_SHAPE_REPRESENTATION('',(#490),#13218);
#459=ADVANCED_BREP_SHAPE_REPRESENTATION('',(#491),#13219);
#460=ADVANCED_BREP_SHAPE_REPRESENTATION('',(#492),#13220);
#461=ADVANCED_BREP_SHAPE_REPRESENTATION('',(#493),#13221);
#462=ADVANCED_BREP_SHAPE_REPRESENTATION('',(#494),#13222);
#463=ADVANCED_BREP_SHAPE_REPRESENTATION('',(#495),#13223);
#464=ADVANCED_BREP_SHAPE_REPRESENTATION('',(#496),#13224);
#465=ADVANCED_BREP_SHAPE_REPRESENTATION('',(#497),#13225);
#466=ADVANCED_BREP_SHAPE_REPRESENTATION('',(#498),#13226);
#467=ADVANCED_BREP_SHAPE_REPRESENTATION('',(#499),#13227);
#468=ADVANCED_BREP_SHAPE_REPRESENTATION('',(#500),#13228);
#469=ADVANCED_BREP_SHAPE_REPRESENTATION('',(#501),#13229);
#470=ADVANCED_BREP_SHAPE_REPRESENTATION('',(#502),#13230);
#471=STYLED_ITEM('',(#13417),#487);
#472=STYLED_ITEM('',(#13418),#488);
#473=STYLED_ITEM('',(#13419),#489);
#474=STYLED_ITEM('',(#13420),#490);
#475=STYLED_ITEM('',(#13421),#491);
#476=STYLED_ITEM('',(#13422),#492);
#477=STYLED_ITEM('',(#13423),#493);
#478=STYLED_ITEM('',(#13417),#494);
#479=STYLED_ITEM('',(#13424),#495);
#480=STYLED_ITEM('',(#13425),#496);
#481=STYLED_ITEM('',(#13426),#497);
#482=STYLED_ITEM('',(#13427),#498);
#483=STYLED_ITEM('',(#13428),#499);
#484=STYLED_ITEM('',(#13422),#500);
#485=STYLED_ITEM('',(#13429),#501);
#486=STYLED_ITEM('',(#13421),#502);
#487=MANIFOLD_SOLID_BREP('Aluminum rectangular hollow profile',#4151);
#488=MANIFOLD_SOLID_BREP('Aluminum square hollow profile',#4152);
#489=MANIFOLD_SOLID_BREP('Body1',#4153);
#490=MANIFOLD_SOLID_BREP('Body1',#4154);
#491=MANIFOLD_SOLID_BREP('Body1',#4155);
#492=MANIFOLD_SOLID_BREP('Body1',#4156);
#493=MANIFOLD_SOLID_BREP('Body1',#4157);
#494=MANIFOLD_SOLID_BREP('Body1',#4158);
#495=MANIFOLD_SOLID_BREP('Body1',#4159);
#496=MANIFOLD_SOLID_BREP('Body1',#4160);
#497=MANIFOLD_SOLID_BREP('Body1',#4161);
#498=MANIFOLD_SOLID_BREP('Body1',#4162);
#499=MANIFOLD_SOLID_BREP('Body1',#4163);
#500=MANIFOLD_SOLID_BREP('Body1',#4164);
#501=MANIFOLD_SOLID_BREP('Body1',#4165);
#502=MANIFOLD_SOLID_BREP('Body1',#4166);
#503=FACE_BOUND('',#857,.T.);
#504=FACE_BOUND('',#873,.T.);
#505=FACE_BOUND('',#877,.T.);
#506=FACE_BOUND('',#893,.T.);
#507=FACE_BOUND('',#903,.T.);
#508=FACE_BOUND('',#904,.T.);
#509=FACE_BOUND('',#905,.T.);
#510=FACE_BOUND('',#906,.T.);
#511=FACE_BOUND('',#908,.T.);
#512=FACE_BOUND('',#909,.T.);
#513=FACE_BOUND('',#910,.T.);
#514=FACE_BOUND('',#911,.T.);
#515=FACE_BOUND('',#921,.T.);
#516=FACE_BOUND('',#922,.T.);
#517=FACE_BOUND('',#923,.T.);
#518=FACE_BOUND('',#924,.T.);
#519=FACE_BOUND('',#926,.T.);
#520=FACE_BOUND('',#927,.T.);
#521=FACE_BOUND('',#928,.T.);
#522=FACE_BOUND('',#929,.T.);
#523=FACE_BOUND('',#947,.T.);
#524=FACE_BOUND('',#948,.T.);
#525=FACE_BOUND('',#949,.T.);
#526=FACE_BOUND('',#950,.T.);
#527=FACE_BOUND('',#953,.T.);
#528=FACE_BOUND('',#954,.T.);
#529=FACE_BOUND('',#955,.T.);
#530=FACE_BOUND('',#956,.T.);
#531=FACE_BOUND('',#1044,.T.);
#532=FACE_BOUND('',#1045,.T.);
#533=FACE_BOUND('',#1046,.T.);
#534=FACE_BOUND('',#1047,.T.);
#535=FACE_BOUND('',#1066,.T.);
#536=FACE_BOUND('',#1067,.T.);
#537=FACE_BOUND('',#1068,.T.);
#538=FACE_BOUND('',#1069,.T.);
#539=FACE_BOUND('',#1079,.T.);
#540=FACE_BOUND('',#1081,.T.);
#541=FACE_BOUND('',#1085,.T.);
#542=FACE_BOUND('',#1087,.T.);
#543=FACE_BOUND('',#1090,.T.);
#544=FACE_BOUND('',#1092,.T.);
#545=FACE_BOUND('',#1095,.T.);
#546=FACE_BOUND('',#1109,.T.);
#547=FACE_BOUND('',#1111,.T.);
#548=FACE_BOUND('',#1115,.T.);
#549=FACE_BOUND('',#1117,.T.);
#550=FACE_BOUND('',#1121,.T.);
#551=FACE_BOUND('',#1123,.T.);
#552=PLANE('',#4349);
#553=PLANE('',#4350);
#554=PLANE('',#4360);
#555=PLANE('',#4367);
#556=PLANE('',#4370);
#557=PLANE('',#4373);
#558=PLANE('',#4376);
#559=PLANE('',#4377);
#560=PLANE('',#4378);
#561=PLANE('',#4379);
#562=PLANE('',#4384);
#563=PLANE('',#4385);
#564=PLANE('',#4395);
#565=PLANE('',#4402);
#566=PLANE('',#4405);
#567=PLANE('',#4408);
#568=PLANE('',#4411);
#569=PLANE('',#4412);
#570=PLANE('',#4413);
#571=PLANE('',#4414);
#572=PLANE('',#4428);
#573=PLANE('',#4429);
#574=PLANE('',#4430);
#575=PLANE('',#4431);
#576=PLANE('',#4432);
#577=PLANE('',#4433);
#578=PLANE('',#4447);
#579=PLANE('',#4448);
#580=PLANE('',#4449);
#581=PLANE('',#4450);
#582=PLANE('',#4451);
#583=PLANE('',#4452);
#584=PLANE('',#4454);
#585=PLANE('',#4455);
#586=PLANE('',#4456);
#587=PLANE('',#4457);
#588=PLANE('',#4458);
#589=PLANE('',#4459);
#590=PLANE('',#4461);
#591=PLANE('',#4462);
#592=PLANE('',#4463);
#593=PLANE('',#4464);
#594=PLANE('',#4465);
#595=PLANE('',#4466);
#596=PLANE('',#4480);
#597=PLANE('',#4481);
#598=PLANE('',#4482);
#599=PLANE('',#4483);
#600=PLANE('',#4484);
#601=PLANE('',#4485);
#602=PLANE('',#4584);
#603=PLANE('',#4592);
#604=PLANE('',#4593);
#605=PLANE('',#4594);
#606=PLANE('',#4595);
#607=PLANE('',#4596);
#608=PLANE('',#4598);
#609=PLANE('',#4599);
#610=PLANE('',#4600);
#611=PLANE('',#4601);
#612=PLANE('',#4602);
#613=PLANE('',#4603);
#614=PLANE('',#4611);
#615=PLANE('',#4612);
#616=PLANE('',#4620);
#617=PLANE('',#4621);
#618=PLANE('',#4626);
#619=PLANE('',#4628);
#620=PLANE('',#4632);
#621=PLANE('',#4637);
#622=PLANE('',#4639);
#623=PLANE('',#4641);
#624=PLANE('',#4642);
#625=PLANE('',#4643);
#626=PLANE('',#4650);
#627=PLANE('',#4658);
#628=PLANE('',#4659);
#629=PLANE('',#4667);
#630=PLANE('',#4668);
#631=PLANE('',#4676);
#632=PLANE('',#4677);
#633=FACE_OUTER_BOUND('',#854,.T.);
#634=FACE_OUTER_BOUND('',#855,.T.);
#635=FACE_OUTER_BOUND('',#856,.T.);
#636=FACE_OUTER_BOUND('',#858,.T.);
#637=FACE_OUTER_BOUND('',#859,.T.);
#638=FACE_OUTER_BOUND('',#860,.T.);
#639=FACE_OUTER_BOUND('',#861,.T.);
#640=FACE_OUTER_BOUND('',#862,.T.);
#641=FACE_OUTER_BOUND('',#863,.T.);
#642=FACE_OUTER_BOUND('',#864,.T.);
#643=FACE_OUTER_BOUND('',#865,.T.);
#644=FACE_OUTER_BOUND('',#866,.T.);
#645=FACE_OUTER_BOUND('',#867,.T.);
#646=FACE_OUTER_BOUND('',#868,.T.);
#647=FACE_OUTER_BOUND('',#869,.T.);
#648=FACE_OUTER_BOUND('',#870,.T.);
#649=FACE_OUTER_BOUND('',#871,.T.);
#650=FACE_OUTER_BOUND('',#872,.T.);
#651=FACE_OUTER_BOUND('',#874,.T.);
#652=FACE_OUTER_BOUND('',#875,.T.);
#653=FACE_OUTER_BOUND('',#876,.T.);
#654=FACE_OUTER_BOUND('',#878,.T.);
#655=FACE_OUTER_BOUND('',#879,.T.);
#656=FACE_OUTER_BOUND('',#880,.T.);
#657=FACE_OUTER_BOUND('',#881,.T.);
#658=FACE_OUTER_BOUND('',#882,.T.);
#659=FACE_OUTER_BOUND('',#883,.T.);
#660=FACE_OUTER_BOUND('',#884,.T.);
#661=FACE_OUTER_BOUND('',#885,.T.);
#662=FACE_OUTER_BOUND('',#886,.T.);
#663=FACE_OUTER_BOUND('',#887,.T.);
#664=FACE_OUTER_BOUND('',#888,.T.);
#665=FACE_OUTER_BOUND('',#889,.T.);
#666=FACE_OUTER_BOUND('',#890,.T.);
#667=FACE_OUTER_BOUND('',#891,.T.);
#668=FACE_OUTER_BOUND('',#892,.T.);
#669=FACE_OUTER_BOUND('',#894,.T.);
#670=FACE_OUTER_BOUND('',#895,.T.);
#671=FACE_OUTER_BOUND('',#896,.T.);
#672=FACE_OUTER_BOUND('',#897,.T.);
#673=FACE_OUTER_BOUND('',#898,.T.);
#674=FACE_OUTER_BOUND('',#899,.T.);
#675=FACE_OUTER_BOUND('',#900,.T.);
#676=FACE_OUTER_BOUND('',#901,.T.);
#677=FACE_OUTER_BOUND('',#902,.T.);
#678=FACE_OUTER_BOUND('',#907,.T.);
#679=FACE_OUTER_BOUND('',#912,.T.);
#680=FACE_OUTER_BOUND('',#913,.T.);
#681=FACE_OUTER_BOUND('',#914,.T.);
#682=FACE_OUTER_BOUND('',#915,.T.);
#683=FACE_OUTER_BOUND('',#916,.T.);
#684=FACE_OUTER_BOUND('',#917,.T.);
#685=FACE_OUTER_BOUND('',#918,.T.);
#686=FACE_OUTER_BOUND('',#919,.T.);
#687=FACE_OUTER_BOUND('',#920,.T.);
#688=FACE_OUTER_BOUND('',#925,.T.);
#689=FACE_OUTER_BOUND('',#930,.T.);
#690=FACE_OUTER_BOUND('',#931,.T.);
#691=FACE_OUTER_BOUND('',#932,.T.);
#692=FACE_OUTER_BOUND('',#933,.T.);
#693=FACE_OUTER_BOUND('',#934,.T.);
#694=FACE_OUTER_BOUND('',#935,.T.);
#695=FACE_OUTER_BOUND('',#936,.T.);
#696=FACE_OUTER_BOUND('',#937,.T.);
#697=FACE_OUTER_BOUND('',#938,.T.);
#698=FACE_OUTER_BOUND('',#939,.T.);
#699=FACE_OUTER_BOUND('',#940,.T.);
#700=FACE_OUTER_BOUND('',#941,.T.);
#701=FACE_OUTER_BOUND('',#942,.T.);
#702=FACE_OUTER_BOUND('',#943,.T.);
#703=FACE_OUTER_BOUND('',#944,.T.);
#704=FACE_OUTER_BOUND('',#945,.T.);
#705=FACE_OUTER_BOUND('',#946,.T.);
#706=FACE_OUTER_BOUND('',#951,.T.);
#707=FACE_OUTER_BOUND('',#952,.T.);
#708=FACE_OUTER_BOUND('',#957,.T.);
#709=FACE_OUTER_BOUND('',#958,.T.);
#710=FACE_OUTER_BOUND('',#959,.T.);
#711=FACE_OUTER_BOUND('',#960,.T.);
#712=FACE_OUTER_BOUND('',#961,.T.);
#713=FACE_OUTER_BOUND('',#962,.T.);
#714=FACE_OUTER_BOUND('',#963,.T.);
#715=FACE_OUTER_BOUND('',#964,.T.);
#716=FACE_OUTER_BOUND('',#965,.T.);
#717=FACE_OUTER_BOUND('',#966,.T.);
#718=FACE_OUTER_BOUND('',#967,.T.);
#719=FACE_OUTER_BOUND('',#968,.T.);
#720=FACE_OUTER_BOUND('',#969,.T.);
#721=FACE_OUTER_BOUND('',#970,.T.);
#722=FACE_OUTER_BOUND('',#971,.T.);
#723=FACE_OUTER_BOUND('',#972,.T.);
#724=FACE_OUTER_BOUND('',#973,.T.);
#725=FACE_OUTER_BOUND('',#974,.T.);
#726=FACE_OUTER_BOUND('',#975,.T.);
#727=FACE_OUTER_BOUND('',#976,.T.);
#728=FACE_OUTER_BOUND('',#977,.T.);
#729=FACE_OUTER_BOUND('',#978,.T.);
#730=FACE_OUTER_BOUND('',#979,.T.);
#731=FACE_OUTER_BOUND('',#980,.T.);
#732=FACE_OUTER_BOUND('',#981,.T.);
#733=FACE_OUTER_BOUND('',#982,.T.);
#734=FACE_OUTER_BOUND('',#983,.T.);
#735=FACE_OUTER_BOUND('',#984,.T.);
#736=FACE_OUTER_BOUND('',#985,.T.);
#737=FACE_OUTER_BOUND('',#986,.T.);
#738=FACE_OUTER_BOUND('',#987,.T.);
#739=FACE_OUTER_BOUND('',#988,.T.);
#740=FACE_OUTER_BOUND('',#989,.T.);
#741=FACE_OUTER_BOUND('',#990,.T.);
#742=FACE_OUTER_BOUND('',#991,.T.);
#743=FACE_OUTER_BOUND('',#992,.T.);
#744=FACE_OUTER_BOUND('',#993,.T.);
#745=FACE_OUTER_BOUND('',#994,.T.);
#746=FACE_OUTER_BOUND('',#995,.T.);
#747=FACE_OUTER_BOUND('',#996,.T.);
#748=FACE_OUTER_BOUND('',#997,.T.);
#749=FACE_OUTER_BOUND('',#998,.T.);
#750=FACE_OUTER_BOUND('',#999,.T.);
#751=FACE_OUTER_BOUND('',#1000,.T.);
#752=FACE_OUTER_BOUND('',#1001,.T.);
#753=FACE_OUTER_BOUND('',#1002,.T.);
#754=FACE_OUTER_BOUND('',#1003,.T.);
#755=FACE_OUTER_BOUND('',#1004,.T.);
#756=FACE_OUTER_BOUND('',#1005,.T.);
#757=FACE_OUTER_BOUND('',#1006,.T.);
#758=FACE_OUTER_BOUND('',#1007,.T.);
#759=FACE_OUTER_BOUND('',#1008,.T.);
#760=FACE_OUTER_BOUND('',#1009,.T.);
#761=FACE_OUTER_BOUND('',#1010,.T.);
#762=FACE_OUTER_BOUND('',#1011,.T.);
#763=FACE_OUTER_BOUND('',#1012,.T.);
#764=FACE_OUTER_BOUND('',#1013,.T.);
#765=FACE_OUTER_BOUND('',#1014,.T.);
#766=FACE_OUTER_BOUND('',#1015,.T.);
#767=FACE_OUTER_BOUND('',#1016,.T.);
#768=FACE_OUTER_BOUND('',#1017,.T.);
#769=FACE_OUTER_BOUND('',#1018,.T.);
#770=FACE_OUTER_BOUND('',#1019,.T.);
#771=FACE_OUTER_BOUND('',#1020,.T.);
#772=FACE_OUTER_BOUND('',#1021,.T.);
#773=FACE_OUTER_BOUND('',#1022,.T.);
#774=FACE_OUTER_BOUND('',#1023,.T.);
#775=FACE_OUTER_BOUND('',#1024,.T.);
#776=FACE_OUTER_BOUND('',#1025,.T.);
#777=FACE_OUTER_BOUND('',#1026,.T.);
#778=FACE_OUTER_BOUND('',#1027,.T.);
#779=FACE_OUTER_BOUND('',#1028,.T.);
#780=FACE_OUTER_BOUND('',#1029,.T.);
#781=FACE_OUTER_BOUND('',#1030,.T.);
#782=FACE_OUTER_BOUND('',#1031,.T.);
#783=FACE_OUTER_BOUND('',#1032,.T.);
#784=FACE_OUTER_BOUND('',#1033,.T.);
#785=FACE_OUTER_BOUND('',#1034,.T.);
#786=FACE_OUTER_BOUND('',#1035,.T.);
#787=FACE_OUTER_BOUND('',#1036,.T.);
#788=FACE_OUTER_BOUND('',#1037,.T.);
#789=FACE_OUTER_BOUND('',#1038,.T.);
#790=FACE_OUTER_BOUND('',#1039,.T.);
#791=FACE_OUTER_BOUND('',#1040,.T.);
#792=FACE_OUTER_BOUND('',#1041,.T.);
#793=FACE_OUTER_BOUND('',#1042,.T.);
#794=FACE_OUTER_BOUND('',#1043,.T.);
#795=FACE_OUTER_BOUND('',#1048,.T.);
#796=FACE_OUTER_BOUND('',#1049,.T.);
#797=FACE_OUTER_BOUND('',#1050,.T.);
#798=FACE_OUTER_BOUND('',#1051,.T.);
#799=FACE_OUTER_BOUND('',#1052,.T.);
#800=FACE_OUTER_BOUND('',#1053,.T.);
#801=FACE_OUTER_BOUND('',#1054,.T.);
#802=FACE_OUTER_BOUND('',#1055,.T.);
#803=FACE_OUTER_BOUND('',#1056,.T.);
#804=FACE_OUTER_BOUND('',#1057,.T.);
#805=FACE_OUTER_BOUND('',#1058,.T.);
#806=FACE_OUTER_BOUND('',#1059,.T.);
#807=FACE_OUTER_BOUND('',#1060,.T.);
#808=FACE_OUTER_BOUND('',#1061,.T.);
#809=FACE_OUTER_BOUND('',#1062,.T.);
#810=FACE_OUTER_BOUND('',#1063,.T.);
#811=FACE_OUTER_BOUND('',#1064,.T.);
#812=FACE_OUTER_BOUND('',#1065,.T.);
#813=FACE_OUTER_BOUND('',#1070,.T.);
#814=FACE_OUTER_BOUND('',#1071,.T.);
#815=FACE_OUTER_BOUND('',#1072,.T.);
#816=FACE_OUTER_BOUND('',#1073,.T.);
#817=FACE_OUTER_BOUND('',#1074,.T.);
#818=FACE_OUTER_BOUND('',#1075,.T.);
#819=FACE_OUTER_BOUND('',#1076,.T.);
#820=FACE_OUTER_BOUND('',#1077,.T.);
#821=FACE_OUTER_BOUND('',#1078,.T.);
#822=FACE_OUTER_BOUND('',#1080,.T.);
#823=FACE_OUTER_BOUND('',#1082,.T.);
#824=FACE_OUTER_BOUND('',#1083,.T.);
#825=FACE_OUTER_BOUND('',#1084,.T.);
#826=FACE_OUTER_BOUND('',#1086,.T.);
#827=FACE_OUTER_BOUND('',#1088,.T.);
#828=FACE_OUTER_BOUND('',#1089,.T.);
#829=FACE_OUTER_BOUND('',#1091,.T.);
#830=FACE_OUTER_BOUND('',#1093,.T.);
#831=FACE_OUTER_BOUND('',#1094,.T.);
#832=FACE_OUTER_BOUND('',#1096,.T.);
#833=FACE_OUTER_BOUND('',#1097,.T.);
#834=FACE_OUTER_BOUND('',#1098,.T.);
#835=FACE_OUTER_BOUND('',#1099,.T.);
#836=FACE_OUTER_BOUND('',#1100,.T.);
#837=FACE_OUTER_BOUND('',#1101,.T.);
#838=FACE_OUTER_BOUND('',#1102,.T.);
#839=FACE_OUTER_BOUND('',#1103,.T.);
#840=FACE_OUTER_BOUND('',#1104,.T.);
#841=FACE_OUTER_BOUND('',#1105,.T.);
#842=FACE_OUTER_BOUND('',#1106,.T.);
#843=FACE_OUTER_BOUND('',#1107,.T.);
#844=FACE_OUTER_BOUND('',#1108,.T.);
#845=FACE_OUTER_BOUND('',#1110,.T.);
#846=FACE_OUTER_BOUND('',#1112,.T.);
#847=FACE_OUTER_BOUND('',#1113,.T.);
#848=FACE_OUTER_BOUND('',#1114,.T.);
#849=FACE_OUTER_BOUND('',#1116,.T.);
#850=FACE_OUTER_BOUND('',#1118,.T.);
#851=FACE_OUTER_BOUND('',#1119,.T.);
#852=FACE_OUTER_BOUND('',#1120,.T.);
#853=FACE_OUTER_BOUND('',#1122,.T.);
#854=EDGE_LOOP('',(#2682,#2683,#2684,#2685));
#855=EDGE_LOOP('',(#2686,#2687,#2688,#2689));
#856=EDGE_LOOP('',(#2690,#2691,#2692,#2693,#2694,#2695,#2696,#2697));
#857=EDGE_LOOP('',(#2698,#2699,#2700,#2701,#2702,#2703,#2704,#2705));
#858=EDGE_LOOP('',(#2706,#2707,#2708,#2709));
#859=EDGE_LOOP('',(#2710,#2711,#2712,#2713));
#860=EDGE_LOOP('',(#2714,#2715,#2716,#2717));
#861=EDGE_LOOP('',(#2718,#2719,#2720,#2721));
#862=EDGE_LOOP('',(#2722,#2723,#2724,#2725));
#863=EDGE_LOOP('',(#2726,#2727,#2728,#2729));
#864=EDGE_LOOP('',(#2730,#2731,#2732,#2733));
#865=EDGE_LOOP('',(#2734,#2735,#2736,#2737));
#866=EDGE_LOOP('',(#2738,#2739,#2740,#2741));
#867=EDGE_LOOP('',(#2742,#2743,#2744,#2745));
#868=EDGE_LOOP('',(#2746,#2747,#2748,#2749));
#869=EDGE_LOOP('',(#2750,#2751,#2752,#2753));
#870=EDGE_LOOP('',(#2754,#2755,#2756,#2757));
#871=EDGE_LOOP('',(#2758,#2759,#2760,#2761));
#872=EDGE_LOOP('',(#2762,#2763,#2764,#2765,#2766,#2767,#2768,#2769));
#873=EDGE_LOOP('',(#2770,#2771,#2772,#2773,#2774,#2775,#2776,#2777));
#874=EDGE_LOOP('',(#2778,#2779,#2780,#2781));
#875=EDGE_LOOP('',(#2782,#2783,#2784,#2785));
#876=EDGE_LOOP('',(#2786,#2787,#2788,#2789,#2790,#2791,#2792,#2793));
#877=EDGE_LOOP('',(#2794,#2795,#2796,#2797,#2798,#2799,#2800,#2801));
#878=EDGE_LOOP('',(#2802,#2803,#2804,#2805));
#879=EDGE_LOOP('',(#2806,#2807,#2808,#2809));
#880=EDGE_LOOP('',(#2810,#2811,#2812,#2813));
#881=EDGE_LOOP('',(#2814,#2815,#2816,#2817));
#882=EDGE_LOOP('',(#2818,#2819,#2820,#2821));
#883=EDGE_LOOP('',(#2822,#2823,#2824,#2825));
#884=EDGE_LOOP('',(#2826,#2827,#2828,#2829));
#885=EDGE_LOOP('',(#2830,#2831,#2832,#2833));
#886=EDGE_LOOP('',(#2834,#2835,#2836,#2837));
#887=EDGE_LOOP('',(#2838,#2839,#2840,#2841));
#888=EDGE_LOOP('',(#2842,#2843,#2844,#2845));
#889=EDGE_LOOP('',(#2846,#2847,#2848,#2849));
#890=EDGE_LOOP('',(#2850,#2851,#2852,#2853));
#891=EDGE_LOOP('',(#2854,#2855,#2856,#2857));
#892=EDGE_LOOP('',(#2858,#2859,#2860,#2861,#2862,#2863,#2864,#2865));
#893=EDGE_LOOP('',(#2866,#2867,#2868,#2869,#2870,#2871,#2872,#2873));
#894=EDGE_LOOP('',(#2874,#2875,#2876,#2877));
#895=EDGE_LOOP('',(#2878,#2879,#2880,#2881));
#896=EDGE_LOOP('',(#2882,#2883,#2884,#2885));
#897=EDGE_LOOP('',(#2886,#2887,#2888,#2889));
#898=EDGE_LOOP('',(#2890,#2891,#2892,#2893));
#899=EDGE_LOOP('',(#2894,#2895,#2896,#2897));
#900=EDGE_LOOP('',(#2898,#2899,#2900,#2901));
#901=EDGE_LOOP('',(#2902,#2903,#2904,#2905));
#902=EDGE_LOOP('',(#2906,#2907,#2908,#2909));
#903=EDGE_LOOP('',(#2910));
#904=EDGE_LOOP('',(#2911));
#905=EDGE_LOOP('',(#2912));
#906=EDGE_LOOP('',(#2913));
#907=EDGE_LOOP('',(#2914,#2915,#2916,#2917));
#908=EDGE_LOOP('',(#2918));
#909=EDGE_LOOP('',(#2919));
#910=EDGE_LOOP('',(#2920));
#911=EDGE_LOOP('',(#2921));
#912=EDGE_LOOP('',(#2922,#2923,#2924,#2925));
#913=EDGE_LOOP('',(#2926,#2927,#2928,#2929));
#914=EDGE_LOOP('',(#2930,#2931,#2932,#2933));
#915=EDGE_LOOP('',(#2934,#2935,#2936,#2937));
#916=EDGE_LOOP('',(#2938,#2939,#2940,#2941));
#917=EDGE_LOOP('',(#2942,#2943,#2944,#2945));
#918=EDGE_LOOP('',(#2946,#2947,#2948,#2949));
#919=EDGE_LOOP('',(#2950,#2951,#2952,#2953));
#920=EDGE_LOOP('',(#2954,#2955,#2956,#2957));
#921=EDGE_LOOP('',(#2958));
#922=EDGE_LOOP('',(#2959));
#923=EDGE_LOOP('',(#2960));
#924=EDGE_LOOP('',(#2961));
#925=EDGE_LOOP('',(#2962,#2963,#2964,#2965));
#926=EDGE_LOOP('',(#2966));
#927=EDGE_LOOP('',(#2967));
#928=EDGE_LOOP('',(#2968));
#929=EDGE_LOOP('',(#2969));
#930=EDGE_LOOP('',(#2970,#2971,#2972,#2973));
#931=EDGE_LOOP('',(#2974,#2975,#2976,#2977));
#932=EDGE_LOOP('',(#2978,#2979,#2980,#2981));
#933=EDGE_LOOP('',(#2982,#2983,#2984,#2985));
#934=EDGE_LOOP('',(#2986,#2987,#2988,#2989));
#935=EDGE_LOOP('',(#2990,#2991,#2992,#2993));
#936=EDGE_LOOP('',(#2994,#2995,#2996,#2997));
#937=EDGE_LOOP('',(#2998,#2999,#3000,#3001));
#938=EDGE_LOOP('',(#3002,#3003,#3004,#3005));
#939=EDGE_LOOP('',(#3006,#3007,#3008,#3009));
#940=EDGE_LOOP('',(#3010,#3011,#3012,#3013));
#941=EDGE_LOOP('',(#3014,#3015,#3016,#3017));
#942=EDGE_LOOP('',(#3018,#3019,#3020,#3021));
#943=EDGE_LOOP('',(#3022,#3023,#3024,#3025));
#944=EDGE_LOOP('',(#3026,#3027,#3028,#3029));
#945=EDGE_LOOP('',(#3030,#3031,#3032,#3033));
#946=EDGE_LOOP('',(#3034,#3035,#3036,#3037));
#947=EDGE_LOOP('',(#3038));
#948=EDGE_LOOP('',(#3039));
#949=EDGE_LOOP('',(#3040));
#950=EDGE_LOOP('',(#3041));
#951=EDGE_LOOP('',(#3042,#3043,#3044,#3045));
#952=EDGE_LOOP('',(#3046,#3047,#3048,#3049));
#953=EDGE_LOOP('',(#3050));
#954=EDGE_LOOP('',(#3051));
#955=EDGE_LOOP('',(#3052));
#956=EDGE_LOOP('',(#3053));
#957=EDGE_LOOP('',(#3054,#3055,#3056,#3057));
#958=EDGE_LOOP('',(#3058,#3059,#3060,#3061));
#959=EDGE_LOOP('',(#3062,#3063,#3064,#3065));
#960=EDGE_LOOP('',(#3066,#3067,#3068,#3069));
#961=EDGE_LOOP('',(#3070,#3071,#3072,#3073));
#962=EDGE_LOOP('',(#3074,#3075,#3076,#3077));
#963=EDGE_LOOP('',(#3078,#3079,#3080,#3081));
#964=EDGE_LOOP('',(#3082,#3083,#3084,#3085));
#965=EDGE_LOOP('',(#3086,#3087,#3088,#3089));
#966=EDGE_LOOP('',(#3090,#3091,#3092,#3093));
#967=EDGE_LOOP('',(#3094,#3095,#3096,#3097));
#968=EDGE_LOOP('',(#3098,#3099,#3100,#3101));
#969=EDGE_LOOP('',(#3102,#3103,#3104,#3105));
#970=EDGE_LOOP('',(#3106,#3107,#3108,#3109));
#971=EDGE_LOOP('',(#3110,#3111,#3112,#3113));
#972=EDGE_LOOP('',(#3114,#3115,#3116,#3117));
#973=EDGE_LOOP('',(#3118,#3119,#3120,#3121));
#974=EDGE_LOOP('',(#3122,#3123,#3124,#3125));
#975=EDGE_LOOP('',(#3126,#3127,#3128,#3129));
#976=EDGE_LOOP('',(#3130,#3131,#3132,#3133));
#977=EDGE_LOOP('',(#3134,#3135,#3136,#3137));
#978=EDGE_LOOP('',(#3138,#3139,#3140,#3141));
#979=EDGE_LOOP('',(#3142,#3143,#3144,#3145));
#980=EDGE_LOOP('',(#3146,#3147,#3148,#3149));
#981=EDGE_LOOP('',(#3150,#3151,#3152,#3153));
#982=EDGE_LOOP('',(#3154,#3155,#3156,#3157));
#983=EDGE_LOOP('',(#3158,#3159,#3160,#3161));
#984=EDGE_LOOP('',(#3162,#3163,#3164,#3165));
#985=EDGE_LOOP('',(#3166,#3167,#3168,#3169));
#986=EDGE_LOOP('',(#3170,#3171,#3172,#3173));
#987=EDGE_LOOP('',(#3174,#3175,#3176,#3177));
#988=EDGE_LOOP('',(#3178,#3179,#3180,#3181));
#989=EDGE_LOOP('',(#3182,#3183,#3184,#3185));
#990=EDGE_LOOP('',(#3186,#3187,#3188,#3189));
#991=EDGE_LOOP('',(#3190,#3191,#3192,#3193));
#992=EDGE_LOOP('',(#3194,#3195,#3196,#3197));
#993=EDGE_LOOP('',(#3198,#3199,#3200,#3201));
#994=EDGE_LOOP('',(#3202,#3203,#3204,#3205));
#995=EDGE_LOOP('',(#3206,#3207,#3208,#3209));
#996=EDGE_LOOP('',(#3210,#3211,#3212,#3213));
#997=EDGE_LOOP('',(#3214,#3215,#3216,#3217));
#998=EDGE_LOOP('',(#3218,#3219,#3220,#3221));
#999=EDGE_LOOP('',(#3222,#3223,#3224,#3225));
#1000=EDGE_LOOP('',(#3226,#3227,#3228,#3229));
#1001=EDGE_LOOP('',(#3230,#3231,#3232,#3233));
#1002=EDGE_LOOP('',(#3234,#3235,#3236,#3237));
#1003=EDGE_LOOP('',(#3238,#3239,#3240,#3241));
#1004=EDGE_LOOP('',(#3242,#3243,#3244,#3245));
#1005=EDGE_LOOP('',(#3246,#3247,#3248,#3249));
#1006=EDGE_LOOP('',(#3250,#3251,#3252,#3253));
#1007=EDGE_LOOP('',(#3254,#3255,#3256,#3257));
#1008=EDGE_LOOP('',(#3258,#3259,#3260,#3261));
#1009=EDGE_LOOP('',(#3262,#3263,#3264,#3265));
#1010=EDGE_LOOP('',(#3266,#3267,#3268,#3269));
#1011=EDGE_LOOP('',(#3270,#3271,#3272,#3273));
#1012=EDGE_LOOP('',(#3274,#3275,#3276,#3277));
#1013=EDGE_LOOP('',(#3278,#3279,#3280,#3281));
#1014=EDGE_LOOP('',(#3282,#3283,#3284,#3285));
#1015=EDGE_LOOP('',(#3286,#3287,#3288,#3289));
#1016=EDGE_LOOP('',(#3290,#3291,#3292,#3293));
#1017=EDGE_LOOP('',(#3294,#3295,#3296,#3297));
#1018=EDGE_LOOP('',(#3298,#3299,#3300,#3301));
#1019=EDGE_LOOP('',(#3302,#3303,#3304,#3305));
#1020=EDGE_LOOP('',(#3306,#3307,#3308,#3309));
#1021=EDGE_LOOP('',(#3310,#3311,#3312,#3313));
#1022=EDGE_LOOP('',(#3314,#3315,#3316,#3317));
#1023=EDGE_LOOP('',(#3318,#3319,#3320,#3321));
#1024=EDGE_LOOP('',(#3322,#3323,#3324,#3325));
#1025=EDGE_LOOP('',(#3326,#3327,#3328,#3329));
#1026=EDGE_LOOP('',(#3330,#3331,#3332,#3333));
#1027=EDGE_LOOP('',(#3334,#3335,#3336,#3337));
#1028=EDGE_LOOP('',(#3338,#3339,#3340,#3341));
#1029=EDGE_LOOP('',(#3342,#3343,#3344,#3345));
#1030=EDGE_LOOP('',(#3346,#3347,#3348,#3349));
#1031=EDGE_LOOP('',(#3350,#3351,#3352,#3353));
#1032=EDGE_LOOP('',(#3354,#3355,#3356,#3357));
#1033=EDGE_LOOP('',(#3358,#3359,#3360,#3361));
#1034=EDGE_LOOP('',(#3362,#3363,#3364,#3365));
#1035=EDGE_LOOP('',(#3366,#3367,#3368,#3369));
#1036=EDGE_LOOP('',(#3370,#3371,#3372,#3373));
#1037=EDGE_LOOP('',(#3374,#3375,#3376,#3377));
#1038=EDGE_LOOP('',(#3378,#3379,#3380,#3381));
#1039=EDGE_LOOP('',(#3382,#3383,#3384,#3385));
#1040=EDGE_LOOP('',(#3386,#3387,#3388,#3389));
#1041=EDGE_LOOP('',(#3390,#3391,#3392,#3393,#3394,#3395,#3396,#3397,#3398,
#3399,#3400,#3401,#3402,#3403,#3404,#3405,#3406,#3407,#3408,#3409,#3410,
#3411,#3412,#3413));
#1042=EDGE_LOOP('',(#3414,#3415,#3416,#3417,#3418,#3419,#3420,#3421,#3422,
#3423,#3424,#3425,#3426,#3427,#3428,#3429,#3430,#3431,#3432,#3433,#3434,
#3435,#3436,#3437));
#1043=EDGE_LOOP('',(#3438,#3439,#3440,#3441));
#1044=EDGE_LOOP('',(#3442,#3443,#3444,#3445));
#1045=EDGE_LOOP('',(#3446,#3447,#3448,#3449));
#1046=EDGE_LOOP('',(#3450,#3451,#3452,#3453));
#1047=EDGE_LOOP('',(#3454,#3455,#3456,#3457));
#1048=EDGE_LOOP('',(#3458,#3459,#3460,#3461));
#1049=EDGE_LOOP('',(#3462,#3463,#3464,#3465,#3466,#3467,#3468,#3469,#3470,
#3471,#3472,#3473,#3474,#3475,#3476,#3477,#3478,#3479,#3480,#3481,#3482,
#3483,#3484,#3485));
#1050=EDGE_LOOP('',(#3486,#3487,#3488,#3489,#3490,#3491,#3492,#3493,#3494,
#3495,#3496,#3497,#3498,#3499,#3500,#3501,#3502,#3503,#3504,#3505,#3506,
#3507,#3508,#3509));
#1051=EDGE_LOOP('',(#3510,#3511,#3512,#3513));
#1052=EDGE_LOOP('',(#3514,#3515,#3516,#3517,#3518,#3519,#3520,#3521,#3522,
#3523,#3524,#3525,#3526,#3527,#3528,#3529,#3530,#3531,#3532,#3533,#3534,
#3535,#3536,#3537));
#1053=EDGE_LOOP('',(#3538,#3539,#3540,#3541,#3542,#3543,#3544,#3545,#3546,
#3547,#3548,#3549,#3550,#3551,#3552,#3553,#3554,#3555,#3556,#3557,#3558,
#3559,#3560,#3561));
#1054=EDGE_LOOP('',(#3562,#3563,#3564,#3565));
#1055=EDGE_LOOP('',(#3566,#3567,#3568,#3569,#3570,#3571,#3572,#3573,#3574,
#3575,#3576,#3577,#3578,#3579,#3580,#3581,#3582,#3583,#3584,#3585,#3586,
#3587,#3588,#3589));
#1056=EDGE_LOOP('',(#3590,#3591,#3592,#3593,#3594,#3595,#3596,#3597,#3598,
#3599,#3600,#3601,#3602,#3603,#3604,#3605,#3606,#3607,#3608,#3609,#3610,
#3611,#3612,#3613));
#1057=EDGE_LOOP('',(#3614,#3615,#3616,#3617));
#1058=EDGE_LOOP('',(#3618,#3619,#3620,#3621));
#1059=EDGE_LOOP('',(#3622,#3623,#3624,#3625));
#1060=EDGE_LOOP('',(#3626,#3627,#3628,#3629));
#1061=EDGE_LOOP('',(#3630,#3631,#3632,#3633));
#1062=EDGE_LOOP('',(#3634,#3635,#3636,#3637));
#1063=EDGE_LOOP('',(#3638,#3639,#3640,#3641));
#1064=EDGE_LOOP('',(#3642,#3643,#3644,#3645));
#1065=EDGE_LOOP('',(#3646,#3647,#3648,#3649));
#1066=EDGE_LOOP('',(#3650,#3651,#3652,#3653));
#1067=EDGE_LOOP('',(#3654,#3655,#3656,#3657));
#1068=EDGE_LOOP('',(#3658,#3659,#3660,#3661));
#1069=EDGE_LOOP('',(#3662,#3663,#3664,#3665));
#1070=EDGE_LOOP('',(#3666,#3667,#3668,#3669));
#1071=EDGE_LOOP('',(#3670,#3671,#3672,#3673));
#1072=EDGE_LOOP('',(#3674,#3675,#3676,#3677));
#1073=EDGE_LOOP('',(#3678,#3679,#3680,#3681));
#1074=EDGE_LOOP('',(#3682,#3683,#3684,#3685));
#1075=EDGE_LOOP('',(#3686,#3687,#3688,#3689));
#1076=EDGE_LOOP('',(#3690,#3691,#3692,#3693));
#1077=EDGE_LOOP('',(#3694,#3695,#3696,#3697));
#1078=EDGE_LOOP('',(#3698));
#1079=EDGE_LOOP('',(#3699));
#1080=EDGE_LOOP('',(#3700));
#1081=EDGE_LOOP('',(#3701));
#1082=EDGE_LOOP('',(#3702,#3703,#3704,#3705));
#1083=EDGE_LOOP('',(#3706,#3707,#3708,#3709));
#1084=EDGE_LOOP('',(#3710));
#1085=EDGE_LOOP('',(#3711));
#1086=EDGE_LOOP('',(#3712));
#1087=EDGE_LOOP('',(#3713));
#1088=EDGE_LOOP('',(#3714,#3715,#3716,#3717));
#1089=EDGE_LOOP('',(#3718));
#1090=EDGE_LOOP('',(#3719));
#1091=EDGE_LOOP('',(#3720));
#1092=EDGE_LOOP('',(#3721));
#1093=EDGE_LOOP('',(#3722,#3723,#3724,#3725));
#1094=EDGE_LOOP('',(#3726));
#1095=EDGE_LOOP('',(#3727));
#1096=EDGE_LOOP('',(#3728,#3729,#3730,#3731));
#1097=EDGE_LOOP('',(#3732));
#1098=EDGE_LOOP('',(#3733,#3734,#3735,#3736));
#1099=EDGE_LOOP('',(#3737));
#1100=EDGE_LOOP('',(#3738,#3739,#3740,#3741));
#1101=EDGE_LOOP('',(#3742,#3743,#3744,#3745));
#1102=EDGE_LOOP('',(#3746,#3747,#3748,#3749));
#1103=EDGE_LOOP('',(#3750,#3751,#3752,#3753));
#1104=EDGE_LOOP('',(#3754,#3755,#3756,#3757));
#1105=EDGE_LOOP('',(#3758,#3759,#3760,#3761));
#1106=EDGE_LOOP('',(#3762,#3763,#3764,#3765));
#1107=EDGE_LOOP('',(#3766,#3767,#3768,#3769));
#1108=EDGE_LOOP('',(#3770));
#1109=EDGE_LOOP('',(#3771));
#1110=EDGE_LOOP('',(#3772));
#1111=EDGE_LOOP('',(#3773));
#1112=EDGE_LOOP('',(#3774,#3775,#3776,#3777));
#1113=EDGE_LOOP('',(#3778,#3779,#3780,#3781));
#1114=EDGE_LOOP('',(#3782));
#1115=EDGE_LOOP('',(#3783));
#1116=EDGE_LOOP('',(#3784));
#1117=EDGE_LOOP('',(#3785));
#1118=EDGE_LOOP('',(#3786,#3787,#3788,#3789));
#1119=EDGE_LOOP('',(#3790,#3791,#3792,#3793));
#1120=EDGE_LOOP('',(#3794));
#1121=EDGE_LOOP('',(#3795));
#1122=EDGE_LOOP('',(#3796));
#1123=EDGE_LOOP('',(#3797));
#1124=LINE('',#5786,#1386);
#1125=LINE('',#5789,#1387);
#1126=LINE('',#5792,#1388);
#1127=LINE('',#5794,#1389);
#1128=LINE('',#5795,#1390);
#1129=LINE('',#5798,#1391);
#1130=LINE('',#5802,#1392);
#1131=LINE('',#5806,#1393);
#1132=LINE('',#5810,#1394);
#1133=LINE('',#5814,#1395);
#1134=LINE('',#5818,#1396);
#1135=LINE('',#5822,#1397);
#1136=LINE('',#5826,#1398);
#1137=LINE('',#5829,#1399);
#1138=LINE('',#5832,#1400);
#1139=LINE('',#5833,#1401);
#1140=LINE('',#5837,#1402);
#1141=LINE('',#5840,#1403);
#1142=LINE('',#5846,#1404);
#1143=LINE('',#5847,#1405);
#1144=LINE('',#5850,#1406);
#1145=LINE('',#5851,#1407);
#1146=LINE('',#5855,#1408);
#1147=LINE('',#5858,#1409);
#1148=LINE('',#5859,#1410);
#1149=LINE('',#5863,#1411);
#1150=LINE('',#5866,#1412);
#1151=LINE('',#5867,#1413);
#1152=LINE('',#5871,#1414);
#1153=LINE('',#5873,#1415);
#1154=LINE('',#5875,#1416);
#1155=LINE('',#5877,#1417);
#1156=LINE('',#5885,#1418);
#1157=LINE('',#5888,#1419);
#1158=LINE('',#5891,#1420);
#1159=LINE('',#5893,#1421);
#1160=LINE('',#5894,#1422);
#1161=LINE('',#5897,#1423);
#1162=LINE('',#5901,#1424);
#1163=LINE('',#5905,#1425);
#1164=LINE('',#5909,#1426);
#1165=LINE('',#5913,#1427);
#1166=LINE('',#5917,#1428);
#1167=LINE('',#5921,#1429);
#1168=LINE('',#5925,#1430);
#1169=LINE('',#5928,#1431);
#1170=LINE('',#5931,#1432);
#1171=LINE('',#5932,#1433);
#1172=LINE('',#5936,#1434);
#1173=LINE('',#5939,#1435);
#1174=LINE('',#5945,#1436);
#1175=LINE('',#5946,#1437);
#1176=LINE('',#5949,#1438);
#1177=LINE('',#5950,#1439);
#1178=LINE('',#5954,#1440);
#1179=LINE('',#5957,#1441);
#1180=LINE('',#5958,#1442);
#1181=LINE('',#5962,#1443);
#1182=LINE('',#5965,#1444);
#1183=LINE('',#5966,#1445);
#1184=LINE('',#5970,#1446);
#1185=LINE('',#5972,#1447);
#1186=LINE('',#5974,#1448);
#1187=LINE('',#5976,#1449);
#1188=LINE('',#5983,#1450);
#1189=LINE('',#5989,#1451);
#1190=LINE('',#5995,#1452);
#1191=LINE('',#6001,#1453);
#1192=LINE('',#6006,#1454);
#1193=LINE('',#6008,#1455);
#1194=LINE('',#6010,#1456);
#1195=LINE('',#6011,#1457);
#1196=LINE('',#6014,#1458);
#1197=LINE('',#6016,#1459);
#1198=LINE('',#6017,#1460);
#1199=LINE('',#6020,#1461);
#1200=LINE('',#6022,#1462);
#1201=LINE('',#6023,#1463);
#1202=LINE('',#6025,#1464);
#1203=LINE('',#6026,#1465);
#1204=LINE('',#6034,#1466);
#1205=LINE('',#6040,#1467);
#1206=LINE('',#6046,#1468);
#1207=LINE('',#6052,#1469);
#1208=LINE('',#6057,#1470);
#1209=LINE('',#6059,#1471);
#1210=LINE('',#6061,#1472);
#1211=LINE('',#6062,#1473);
#1212=LINE('',#6065,#1474);
#1213=LINE('',#6067,#1475);
#1214=LINE('',#6068,#1476);
#1215=LINE('',#6071,#1477);
#1216=LINE('',#6073,#1478);
#1217=LINE('',#6074,#1479);
#1218=LINE('',#6076,#1480);
#1219=LINE('',#6077,#1481);
#1220=LINE('',#6084,#1482);
#1221=LINE('',#6086,#1483);
#1222=LINE('',#6088,#1484);
#1223=LINE('',#6089,#1485);
#1224=LINE('',#6092,#1486);
#1225=LINE('',#6094,#1487);
#1226=LINE('',#6095,#1488);
#1227=LINE('',#6098,#1489);
#1228=LINE('',#6100,#1490);
#1229=LINE('',#6101,#1491);
#1230=LINE('',#6103,#1492);
#1231=LINE('',#6104,#1493);
#1232=LINE('',#6111,#1494);
#1233=LINE('',#6113,#1495);
#1234=LINE('',#6115,#1496);
#1235=LINE('',#6116,#1497);
#1236=LINE('',#6119,#1498);
#1237=LINE('',#6121,#1499);
#1238=LINE('',#6122,#1500);
#1239=LINE('',#6125,#1501);
#1240=LINE('',#6127,#1502);
#1241=LINE('',#6128,#1503);
#1242=LINE('',#6130,#1504);
#1243=LINE('',#6131,#1505);
#1244=LINE('',#6139,#1506);
#1245=LINE('',#6145,#1507);
#1246=LINE('',#6151,#1508);
#1247=LINE('',#6157,#1509);
#1248=LINE('',#6162,#1510);
#1249=LINE('',#6164,#1511);
#1250=LINE('',#6166,#1512);
#1251=LINE('',#6167,#1513);
#1252=LINE('',#6170,#1514);
#1253=LINE('',#6172,#1515);
#1254=LINE('',#6173,#1516);
#1255=LINE('',#6176,#1517);
#1256=LINE('',#6178,#1518);
#1257=LINE('',#6179,#1519);
#1258=LINE('',#6181,#1520);
#1259=LINE('',#6182,#1521);
#1260=LINE('',#6189,#1522);
#1261=LINE('',#6210,#1523);
#1262=LINE('',#6261,#1524);
#1263=LINE('',#6312,#1525);
#1264=LINE('',#6360,#1526);
#1265=LINE('',#6408,#1527);
#1266=LINE('',#6459,#1528);
#1267=LINE('',#6510,#1529);
#1268=LINE('',#6558,#1530);
#1269=LINE('',#6609,#1531);
#1270=LINE('',#6648,#1532);
#1271=LINE('',#6669,#1533);
#1272=LINE('',#6720,#1534);
#1273=LINE('',#6771,#1535);
#1274=LINE('',#6819,#1536);
#1275=LINE('',#6867,#1537);
#1276=LINE('',#6918,#1538);
#1277=LINE('',#6969,#1539);
#1278=LINE('',#7017,#1540);
#1279=LINE('',#7068,#1541);
#1280=LINE('',#7107,#1542);
#1281=LINE('',#7128,#1543);
#1282=LINE('',#7179,#1544);
#1283=LINE('',#7230,#1545);
#1284=LINE('',#7278,#1546);
#1285=LINE('',#7326,#1547);
#1286=LINE('',#7377,#1548);
#1287=LINE('',#7428,#1549);
#1288=LINE('',#7476,#1550);
#1289=LINE('',#7527,#1551);
#1290=LINE('',#7566,#1552);
#1291=LINE('',#7587,#1553);
#1292=LINE('',#7638,#1554);
#1293=LINE('',#7689,#1555);
#1294=LINE('',#7737,#1556);
#1295=LINE('',#7785,#1557);
#1296=LINE('',#7836,#1558);
#1297=LINE('',#7887,#1559);
#1298=LINE('',#7935,#1560);
#1299=LINE('',#7986,#1561);
#1300=LINE('',#8025,#1562);
#1301=LINE('',#8049,#1563);
#1302=LINE('',#8073,#1564);
#1303=LINE('',#8098,#1565);
#1304=LINE('',#8122,#1566);
#1305=LINE('',#8147,#1567);
#1306=LINE('',#8171,#1568);
#1307=LINE('',#8196,#1569);
#1308=LINE('',#8221,#1570);
#1309=LINE('',#8245,#1571);
#1310=LINE('',#8262,#1572);
#1311=LINE('',#8286,#1573);
#1312=LINE('',#8310,#1574);
#1313=LINE('',#8335,#1575);
#1314=LINE('',#8359,#1576);
#1315=LINE('',#8384,#1577);
#1316=LINE('',#8408,#1578);
#1317=LINE('',#8433,#1579);
#1318=LINE('',#8458,#1580);
#1319=LINE('',#8482,#1581);
#1320=LINE('',#8499,#1582);
#1321=LINE('',#8523,#1583);
#1322=LINE('',#8547,#1584);
#1323=LINE('',#8572,#1585);
#1324=LINE('',#8596,#1586);
#1325=LINE('',#8621,#1587);
#1326=LINE('',#8645,#1588);
#1327=LINE('',#8670,#1589);
#1328=LINE('',#8695,#1590);
#1329=LINE('',#8719,#1591);
#1330=LINE('',#8736,#1592);
#1331=LINE('',#8760,#1593);
#1332=LINE('',#8784,#1594);
#1333=LINE('',#8809,#1595);
#1334=LINE('',#8833,#1596);
#1335=LINE('',#8858,#1597);
#1336=LINE('',#8882,#1598);
#1337=LINE('',#8907,#1599);
#1338=LINE('',#8932,#1600);
#1339=LINE('',#8956,#1601);
#1340=LINE('',#9968,#1602);
#1341=LINE('',#9970,#1603);
#1342=LINE('',#9972,#1604);
#1343=LINE('',#9973,#1605);
#1344=LINE('',#12966,#1606);
#1345=LINE('',#12967,#1607);
#1346=LINE('',#12968,#1608);
#1347=LINE('',#12971,#1609);
#1348=LINE('',#12972,#1610);
#1349=LINE('',#12975,#1611);
#1350=LINE('',#12976,#1612);
#1351=LINE('',#12978,#1613);
#1352=LINE('',#12984,#1614);
#1353=LINE('',#12986,#1615);
#1354=LINE('',#12988,#1616);
#1355=LINE('',#12989,#1617);
#1356=LINE('',#12992,#1618);
#1357=LINE('',#12994,#1619);
#1358=LINE('',#12995,#1620);
#1359=LINE('',#12998,#1621);
#1360=LINE('',#13000,#1622);
#1361=LINE('',#13001,#1623);
#1362=LINE('',#13003,#1624);
#1363=LINE('',#13004,#1625);
#1364=LINE('',#13012,#1626);
#1365=LINE('',#13018,#1627);
#1366=LINE('',#13027,#1628);
#1367=LINE('',#13033,#1629);
#1368=LINE('',#13042,#1630);
#1369=LINE('',#13053,#1631);
#1370=LINE('',#13061,#1632);
#1371=LINE('',#13065,#1633);
#1372=LINE('',#13071,#1634);
#1373=LINE('',#13073,#1635);
#1374=LINE('',#13075,#1636);
#1375=LINE('',#13076,#1637);
#1376=LINE('',#13080,#1638);
#1377=LINE('',#13082,#1639);
#1378=LINE('',#13084,#1640);
#1379=LINE('',#13085,#1641);
#1380=LINE('',#13099,#1642);
#1381=LINE('',#13105,#1643);
#1382=LINE('',#13114,#1644);
#1383=LINE('',#13120,#1645);
#1384=LINE('',#13129,#1646);
#1385=LINE('',#13135,#1647);
#1386=VECTOR('',#4743,10.);
#1387=VECTOR('',#4746,10.);
#1388=VECTOR('',#4749,10.);
#1389=VECTOR('',#4750,10.);
#1390=VECTOR('',#4751,10.);
#1391=VECTOR('',#4754,10.);
#1392=VECTOR('',#4757,10.);
#1393=VECTOR('',#4760,10.);
#1394=VECTOR('',#4763,10.);
#1395=VECTOR('',#4766,10.);
#1396=VECTOR('',#4769,10.);
#1397=VECTOR('',#4772,10.);
#1398=VECTOR('',#4777,10.);
#1399=VECTOR('',#4780,10.);
#1400=VECTOR('',#4783,10.);
#1401=VECTOR('',#4784,10.);
#1402=VECTOR('',#4789,10.);
#1403=VECTOR('',#4792,10.);
#1404=VECTOR('',#4799,10.);
#1405=VECTOR('',#4800,10.);
#1406=VECTOR('',#4803,10.);
#1407=VECTOR('',#4804,10.);
#1408=VECTOR('',#4809,10.);
#1409=VECTOR('',#4812,10.);
#1410=VECTOR('',#4813,10.);
#1411=VECTOR('',#4818,10.);
#1412=VECTOR('',#4821,10.);
#1413=VECTOR('',#4822,10.);
#1414=VECTOR('',#4827,10.);
#1415=VECTOR('',#4830,10.);
#1416=VECTOR('',#4833,10.);
#1417=VECTOR('',#4836,10.);
#1418=VECTOR('',#4845,10.);
#1419=VECTOR('',#4848,10.);
#1420=VECTOR('',#4851,10.);
#1421=VECTOR('',#4852,10.);
#1422=VECTOR('',#4853,10.);
#1423=VECTOR('',#4856,10.);
#1424=VECTOR('',#4859,10.);
#1425=VECTOR('',#4862,10.);
#1426=VECTOR('',#4865,10.);
#1427=VECTOR('',#4868,10.);
#1428=VECTOR('',#4871,10.);
#1429=VECTOR('',#4874,10.);
#1430=VECTOR('',#4879,10.);
#1431=VECTOR('',#4882,10.);
#1432=VECTOR('',#4885,10.);
#1433=VECTOR('',#4886,10.);
#1434=VECTOR('',#4891,10.);
#1435=VECTOR('',#4894,10.);
#1436=VECTOR('',#4901,10.);
#1437=VECTOR('',#4902,10.);
#1438=VECTOR('',#4905,10.);
#1439=VECTOR('',#4906,10.);
#1440=VECTOR('',#4911,10.);
#1441=VECTOR('',#4914,10.);
#1442=VECTOR('',#4915,10.);
#1443=VECTOR('',#4920,10.);
#1444=VECTOR('',#4923,10.);
#1445=VECTOR('',#4924,10.);
#1446=VECTOR('',#4929,10.);
#1447=VECTOR('',#4932,10.);
#1448=VECTOR('',#4935,10.);
#1449=VECTOR('',#4938,10.);
#1450=VECTOR('',#4947,7.);
#1451=VECTOR('',#4954,7.);
#1452=VECTOR('',#4961,7.);
#1453=VECTOR('',#4968,7.);
#1454=VECTOR('',#4973,10.);
#1455=VECTOR('',#4974,10.);
#1456=VECTOR('',#4975,10.);
#1457=VECTOR('',#4976,10.);
#1458=VECTOR('',#4979,10.);
#1459=VECTOR('',#4980,10.);
#1460=VECTOR('',#4981,10.);
#1461=VECTOR('',#4984,10.);
#1462=VECTOR('',#4985,10.);
#1463=VECTOR('',#4986,10.);
#1464=VECTOR('',#4989,10.);
#1465=VECTOR('',#4990,10.);
#1466=VECTOR('',#5001,7.);
#1467=VECTOR('',#5008,7.);
#1468=VECTOR('',#5015,7.);
#1469=VECTOR('',#5022,7.);
#1470=VECTOR('',#5027,10.);
#1471=VECTOR('',#5028,10.);
#1472=VECTOR('',#5029,10.);
#1473=VECTOR('',#5030,10.);
#1474=VECTOR('',#5033,10.);
#1475=VECTOR('',#5034,10.);
#1476=VECTOR('',#5035,10.);
#1477=VECTOR('',#5038,10.);
#1478=VECTOR('',#5039,10.);
#1479=VECTOR('',#5040,10.);
#1480=VECTOR('',#5043,10.);
#1481=VECTOR('',#5044,10.);
#1482=VECTOR('',#5053,10.);
#1483=VECTOR('',#5054,10.);
#1484=VECTOR('',#5055,10.);
#1485=VECTOR('',#5056,10.);
#1486=VECTOR('',#5059,10.);
#1487=VECTOR('',#5060,10.);
#1488=VECTOR('',#5061,10.);
#1489=VECTOR('',#5064,10.);
#1490=VECTOR('',#5065,10.);
#1491=VECTOR('',#5066,10.);
#1492=VECTOR('',#5069,10.);
#1493=VECTOR('',#5070,10.);
#1494=VECTOR('',#5079,10.);
#1495=VECTOR('',#5080,10.);
#1496=VECTOR('',#5081,10.);
#1497=VECTOR('',#5082,10.);
#1498=VECTOR('',#5085,10.);
#1499=VECTOR('',#5086,10.);
#1500=VECTOR('',#5087,10.);
#1501=VECTOR('',#5090,10.);
#1502=VECTOR('',#5091,10.);
#1503=VECTOR('',#5092,10.);
#1504=VECTOR('',#5095,10.);
#1505=VECTOR('',#5096,10.);
#1506=VECTOR('',#5107,6.);
#1507=VECTOR('',#5114,6.);
#1508=VECTOR('',#5121,6.);
#1509=VECTOR('',#5128,6.);
#1510=VECTOR('',#5133,10.);
#1511=VECTOR('',#5134,10.);
#1512=VECTOR('',#5135,10.);
#1513=VECTOR('',#5136,10.);
#1514=VECTOR('',#5139,10.);
#1515=VECTOR('',#5140,10.);
#1516=VECTOR('',#5141,10.);
#1517=VECTOR('',#5144,10.);
#1518=VECTOR('',#5145,10.);
#1519=VECTOR('',#5146,10.);
#1520=VECTOR('',#5149,10.);
#1521=VECTOR('',#5150,10.);
#1522=VECTOR('',#5159,3.);
#1523=VECTOR('',#5164,3.);
#1524=VECTOR('',#5167,3.);
#1525=VECTOR('',#5170,3.);
#1526=VECTOR('',#5173,3.);
#1527=VECTOR('',#5176,3.);
#1528=VECTOR('',#5179,3.);
#1529=VECTOR('',#5182,3.);
#1530=VECTOR('',#5185,3.);
#1531=VECTOR('',#5188,3.);
#1532=VECTOR('',#5193,3.);
#1533=VECTOR('',#5198,3.);
#1534=VECTOR('',#5201,3.);
#1535=VECTOR('',#5204,3.);
#1536=VECTOR('',#5207,3.);
#1537=VECTOR('',#5210,3.);
#1538=VECTOR('',#5213,3.);
#1539=VECTOR('',#5216,3.);
#1540=VECTOR('',#5219,3.);
#1541=VECTOR('',#5222,3.);
#1542=VECTOR('',#5227,3.);
#1543=VECTOR('',#5232,3.);
#1544=VECTOR('',#5235,3.);
#1545=VECTOR('',#5238,3.);
#1546=VECTOR('',#5241,3.);
#1547=VECTOR('',#5244,3.);
#1548=VECTOR('',#5247,3.);
#1549=VECTOR('',#5250,3.);
#1550=VECTOR('',#5253,3.);
#1551=VECTOR('',#5256,3.);
#1552=VECTOR('',#5261,3.);
#1553=VECTOR('',#5266,3.);
#1554=VECTOR('',#5269,3.);
#1555=VECTOR('',#5272,3.);
#1556=VECTOR('',#5275,3.);
#1557=VECTOR('',#5278,3.);
#1558=VECTOR('',#5281,3.);
#1559=VECTOR('',#5284,3.);
#1560=VECTOR('',#5287,3.);
#1561=VECTOR('',#5290,3.);
#1562=VECTOR('',#5295,3.0735);
#1563=VECTOR('',#5300,3.0735);
#1564=VECTOR('',#5303,3.0735);
#1565=VECTOR('',#5306,3.0735);
#1566=VECTOR('',#5309,3.0735);
#1567=VECTOR('',#5312,3.0735);
#1568=VECTOR('',#5315,3.0735);
#1569=VECTOR('',#5318,3.0735);
#1570=VECTOR('',#5321,3.0735);
#1571=VECTOR('',#5324,3.0735);
#1572=VECTOR('',#5329,3.07350000000001);
#1573=VECTOR('',#5334,3.07350000000001);
#1574=VECTOR('',#5337,3.07350000000001);
#1575=VECTOR('',#5340,3.07350000000001);
#1576=VECTOR('',#5343,3.07350000000001);
#1577=VECTOR('',#5346,3.07350000000001);
#1578=VECTOR('',#5349,3.07350000000001);
#1579=VECTOR('',#5352,3.07350000000001);
#1580=VECTOR('',#5355,3.07350000000001);
#1581=VECTOR('',#5358,3.07350000000001);
#1582=VECTOR('',#5363,3.07350000000001);
#1583=VECTOR('',#5368,3.0735);
#1584=VECTOR('',#5371,3.0735);
#1585=VECTOR('',#5374,3.0735);
#1586=VECTOR('',#5377,3.07350000000001);
#1587=VECTOR('',#5380,3.07350000000001);
#1588=VECTOR('',#5383,3.0735);
#1589=VECTOR('',#5386,3.0735);
#1590=VECTOR('',#5389,3.0735);
#1591=VECTOR('',#5392,3.0735);
#1592=VECTOR('',#5397,3.07350000000001);
#1593=VECTOR('',#5402,3.07350000000001);
#1594=VECTOR('',#5405,3.07350000000001);
#1595=VECTOR('',#5408,3.07350000000001);
#1596=VECTOR('',#5411,3.07350000000001);
#1597=VECTOR('',#5414,3.07350000000001);
#1598=VECTOR('',#5417,3.07350000000001);
#1599=VECTOR('',#5420,3.07350000000001);
#1600=VECTOR('',#5423,3.07350000000001);
#1601=VECTOR('',#5426,3.07350000000001);
#1602=VECTOR('',#5433,10.);
#1603=VECTOR('',#5434,10.);
#1604=VECTOR('',#5435,10.);
#1605=VECTOR('',#5436,10.);
#1606=VECTOR('',#5453,10.);
#1607=VECTOR('',#5454,10.);
#1608=VECTOR('',#5455,10.);
#1609=VECTOR('',#5458,10.);
#1610=VECTOR('',#5459,10.);
#1611=VECTOR('',#5462,10.);
#1612=VECTOR('',#5463,10.);
#1613=VECTOR('',#5466,10.);
#1614=VECTOR('',#5473,10.);
#1615=VECTOR('',#5474,10.);
#1616=VECTOR('',#5475,10.);
#1617=VECTOR('',#5476,10.);
#1618=VECTOR('',#5479,10.);
#1619=VECTOR('',#5480,10.);
#1620=VECTOR('',#5481,10.);
#1621=VECTOR('',#5484,10.);
#1622=VECTOR('',#5485,10.);
#1623=VECTOR('',#5486,10.);
#1624=VECTOR('',#5489,10.);
#1625=VECTOR('',#5490,10.);
#1626=VECTOR('',#5501,8.);
#1627=VECTOR('',#5508,15.);
#1628=VECTOR('',#5521,6.);
#1629=VECTOR('',#5528,8.);
#1630=VECTOR('',#5541,5.);
#1631=VECTOR('',#5556,6.);
#1632=VECTOR('',#5565,9.);
#1633=VECTOR('',#5572,6.);
#1634=VECTOR('',#5579,10.);
#1635=VECTOR('',#5580,10.);
#1636=VECTOR('',#5581,10.);
#1637=VECTOR('',#5582,10.);
#1638=VECTOR('',#5585,10.);
#1639=VECTOR('',#5586,10.);
#1640=VECTOR('',#5587,10.);
#1641=VECTOR('',#5588,10.);
#1642=VECTOR('',#5611,6.);
#1643=VECTOR('',#5618,10.);
#1644=VECTOR('',#5631,6.);
#1645=VECTOR('',#5638,11.);
#1646=VECTOR('',#5651,6.);
#1647=VECTOR('',#5658,11.);
#1648=CIRCLE('',#4347,1.);
#1649=CIRCLE('',#4348,1.);
#1650=CIRCLE('',#4351,1.);
#1651=CIRCLE('',#4352,1.);
#1652=CIRCLE('',#4353,1.);
#1653=CIRCLE('',#4354,1.);
#1654=CIRCLE('',#4355,1.);
#1655=CIRCLE('',#4356,1.);
#1656=CIRCLE('',#4357,1.);
#1657=CIRCLE('',#4359,1.);
#1658=CIRCLE('',#4362,1.);
#1659=CIRCLE('',#4364,1.);
#1660=CIRCLE('',#4366,1.);
#1661=CIRCLE('',#4369,1.);
#1662=CIRCLE('',#4372,1.);
#1663=CIRCLE('',#4375,1.);
#1664=CIRCLE('',#4382,1.);
#1665=CIRCLE('',#4383,1.);
#1666=CIRCLE('',#4386,1.);
#1667=CIRCLE('',#4387,1.);
#1668=CIRCLE('',#4388,1.);
#1669=CIRCLE('',#4389,1.);
#1670=CIRCLE('',#4390,1.);
#1671=CIRCLE('',#4391,1.);
#1672=CIRCLE('',#4392,1.);
#1673=CIRCLE('',#4394,1.);
#1674=CIRCLE('',#4397,1.);
#1675=CIRCLE('',#4399,1.);
#1676=CIRCLE('',#4401,1.);
#1677=CIRCLE('',#4404,1.);
#1678=CIRCLE('',#4407,1.);
#1679=CIRCLE('',#4410,1.);
#1680=CIRCLE('',#4417,7.);
#1681=CIRCLE('',#4418,7.);
#1682=CIRCLE('',#4420,7.);
#1683=CIRCLE('',#4421,7.);
#1684=CIRCLE('',#4423,7.);
#1685=CIRCLE('',#4424,7.);
#1686=CIRCLE('',#4426,7.);
#1687=CIRCLE('',#4427,7.);
#1688=CIRCLE('',#4436,7.);
#1689=CIRCLE('',#4437,7.);
#1690=CIRCLE('',#4439,7.);
#1691=CIRCLE('',#4440,7.);
#1692=CIRCLE('',#4442,7.);
#1693=CIRCLE('',#4443,7.);
#1694=CIRCLE('',#4445,7.);
#1695=CIRCLE('',#4446,7.);
#1696=CIRCLE('',#4469,6.);
#1697=CIRCLE('',#4470,6.);
#1698=CIRCLE('',#4472,6.);
#1699=CIRCLE('',#4473,6.);
#1700=CIRCLE('',#4475,6.);
#1701=CIRCLE('',#4476,6.);
#1702=CIRCLE('',#4478,6.);
#1703=CIRCLE('',#4479,6.);
#1704=CIRCLE('',#4488,2.5175);
#1705=CIRCLE('',#4498,2.5175);
#1706=CIRCLE('',#4500,2.5175);
#1707=CIRCLE('',#4510,2.5175);
#1708=CIRCLE('',#4512,2.5175);
#1709=CIRCLE('',#4522,2.5175);
#1710=CIRCLE('',#4524,2.5175);
#1711=CIRCLE('',#4534,2.5175);
#1712=CIRCLE('',#4536,3.07349999999999);
#1713=CIRCLE('',#4546,3.0735);
#1714=CIRCLE('',#4548,3.07350000000001);
#1715=CIRCLE('',#4558,3.07350000000001);
#1716=CIRCLE('',#4560,3.0735);
#1717=CIRCLE('',#4570,3.0735);
#1718=CIRCLE('',#4572,3.07350000000001);
#1719=CIRCLE('',#4582,3.07350000000001);
#1720=CIRCLE('',#4606,8.);
#1721=CIRCLE('',#4607,8.);
#1722=CIRCLE('',#4609,15.);
#1723=CIRCLE('',#4610,15.);
#1724=CIRCLE('',#4615,6.);
#1725=CIRCLE('',#4616,6.);
#1726=CIRCLE('',#4618,8.);
#1727=CIRCLE('',#4619,8.);
#1728=CIRCLE('',#4624,5.);
#1729=CIRCLE('',#4625,5.);
#1730=CIRCLE('',#4627,6.);
#1731=CIRCLE('',#4629,6.);
#1732=CIRCLE('',#4631,6.);
#1733=CIRCLE('',#4633,9.);
#1734=CIRCLE('',#4634,6.);
#1735=CIRCLE('',#4636,9.);
#1736=CIRCLE('',#4644,9.);
#1737=CIRCLE('',#4645,5.);
#1738=CIRCLE('',#4647,5.);
#1739=CIRCLE('',#4649,9.);
#1740=CIRCLE('',#4653,6.);
#1741=CIRCLE('',#4654,6.);
#1742=CIRCLE('',#4656,10.);
#1743=CIRCLE('',#4657,10.);
#1744=CIRCLE('',#4662,6.);
#1745=CIRCLE('',#4663,6.);
#1746=CIRCLE('',#4665,11.);
#1747=CIRCLE('',#4666,11.);
#1748=CIRCLE('',#4671,6.);
#1749=CIRCLE('',#4672,6.);
#1750=CIRCLE('',#4674,11.);
#1751=CIRCLE('',#4675,11.);
#1752=VERTEX_POINT('',#5782);
#1753=VERTEX_POINT('',#5783);
#1754=VERTEX_POINT('',#5785);
#1755=VERTEX_POINT('',#5787);
#1756=VERTEX_POINT('',#5791);
#1757=VERTEX_POINT('',#5793);
#1758=VERTEX_POINT('',#5797);
#1759=VERTEX_POINT('',#5799);
#1760=VERTEX_POINT('',#5801);
#1761=VERTEX_POINT('',#5803);
#1762=VERTEX_POINT('',#5805);
#1763=VERTEX_POINT('',#5808);
#1764=VERTEX_POINT('',#5809);
#1765=VERTEX_POINT('',#5811);
#1766=VERTEX_POINT('',#5813);
#1767=VERTEX_POINT('',#5815);
#1768=VERTEX_POINT('',#5817);
#1769=VERTEX_POINT('',#5819);
#1770=VERTEX_POINT('',#5821);
#1771=VERTEX_POINT('',#5825);
#1772=VERTEX_POINT('',#5827);
#1773=VERTEX_POINT('',#5831);
#1774=VERTEX_POINT('',#5835);
#1775=VERTEX_POINT('',#5839);
#1776=VERTEX_POINT('',#5843);
#1777=VERTEX_POINT('',#5844);
#1778=VERTEX_POINT('',#5849);
#1779=VERTEX_POINT('',#5853);
#1780=VERTEX_POINT('',#5857);
#1781=VERTEX_POINT('',#5861);
#1782=VERTEX_POINT('',#5865);
#1783=VERTEX_POINT('',#5869);
#1784=VERTEX_POINT('',#5881);
#1785=VERTEX_POINT('',#5882);
#1786=VERTEX_POINT('',#5884);
#1787=VERTEX_POINT('',#5886);
#1788=VERTEX_POINT('',#5890);
#1789=VERTEX_POINT('',#5892);
#1790=VERTEX_POINT('',#5896);
#1791=VERTEX_POINT('',#5898);
#1792=VERTEX_POINT('',#5900);
#1793=VERTEX_POINT('',#5902);
#1794=VERTEX_POINT('',#5904);
#1795=VERTEX_POINT('',#5907);
#1796=VERTEX_POINT('',#5908);
#1797=VERTEX_POINT('',#5910);
#1798=VERTEX_POINT('',#5912);
#1799=VERTEX_POINT('',#5914);
#1800=VERTEX_POINT('',#5916);
#1801=VERTEX_POINT('',#5918);
#1802=VERTEX_POINT('',#5920);
#1803=VERTEX_POINT('',#5924);
#1804=VERTEX_POINT('',#5926);
#1805=VERTEX_POINT('',#5930);
#1806=VERTEX_POINT('',#5934);
#1807=VERTEX_POINT('',#5938);
#1808=VERTEX_POINT('',#5942);
#1809=VERTEX_POINT('',#5943);
#1810=VERTEX_POINT('',#5948);
#1811=VERTEX_POINT('',#5952);
#1812=VERTEX_POINT('',#5956);
#1813=VERTEX_POINT('',#5960);
#1814=VERTEX_POINT('',#5964);
#1815=VERTEX_POINT('',#5968);
#1816=VERTEX_POINT('',#5980);
#1817=VERTEX_POINT('',#5982);
#1818=VERTEX_POINT('',#5986);
#1819=VERTEX_POINT('',#5988);
#1820=VERTEX_POINT('',#5992);
#1821=VERTEX_POINT('',#5994);
#1822=VERTEX_POINT('',#5998);
#1823=VERTEX_POINT('',#6000);
#1824=VERTEX_POINT('',#6004);
#1825=VERTEX_POINT('',#6005);
#1826=VERTEX_POINT('',#6007);
#1827=VERTEX_POINT('',#6009);
#1828=VERTEX_POINT('',#6013);
#1829=VERTEX_POINT('',#6015);
#1830=VERTEX_POINT('',#6019);
#1831=VERTEX_POINT('',#6021);
#1832=VERTEX_POINT('',#6031);
#1833=VERTEX_POINT('',#6033);
#1834=VERTEX_POINT('',#6037);
#1835=VERTEX_POINT('',#6039);
#1836=VERTEX_POINT('',#6043);
#1837=VERTEX_POINT('',#6045);
#1838=VERTEX_POINT('',#6049);
#1839=VERTEX_POINT('',#6051);
#1840=VERTEX_POINT('',#6055);
#1841=VERTEX_POINT('',#6056);
#1842=VERTEX_POINT('',#6058);
#1843=VERTEX_POINT('',#6060);
#1844=VERTEX_POINT('',#6064);
#1845=VERTEX_POINT('',#6066);
#1846=VERTEX_POINT('',#6070);
#1847=VERTEX_POINT('',#6072);
#1848=VERTEX_POINT('',#6082);
#1849=VERTEX_POINT('',#6083);
#1850=VERTEX_POINT('',#6085);
#1851=VERTEX_POINT('',#6087);
#1852=VERTEX_POINT('',#6091);
#1853=VERTEX_POINT('',#6093);
#1854=VERTEX_POINT('',#6097);
#1855=VERTEX_POINT('',#6099);
#1856=VERTEX_POINT('',#6109);
#1857=VERTEX_POINT('',#6110);
#1858=VERTEX_POINT('',#6112);
#1859=VERTEX_POINT('',#6114);
#1860=VERTEX_POINT('',#6118);
#1861=VERTEX_POINT('',#6120);
#1862=VERTEX_POINT('',#6124);
#1863=VERTEX_POINT('',#6126);
#1864=VERTEX_POINT('',#6136);
#1865=VERTEX_POINT('',#6138);
#1866=VERTEX_POINT('',#6142);
#1867=VERTEX_POINT('',#6144);
#1868=VERTEX_POINT('',#6148);
#1869=VERTEX_POINT('',#6150);
#1870=VERTEX_POINT('',#6154);
#1871=VERTEX_POINT('',#6156);
#1872=VERTEX_POINT('',#6160);
#1873=VERTEX_POINT('',#6161);
#1874=VERTEX_POINT('',#6163);
#1875=VERTEX_POINT('',#6165);
#1876=VERTEX_POINT('',#6169);
#1877=VERTEX_POINT('',#6171);
#1878=VERTEX_POINT('',#6175);
#1879=VERTEX_POINT('',#6177);
#1880=VERTEX_POINT('',#6187);
#1881=VERTEX_POINT('',#6188);
#1882=VERTEX_POINT('',#6190);
#1883=VERTEX_POINT('',#6195);
#1884=VERTEX_POINT('',#6208);
#1885=VERTEX_POINT('',#6209);
#1886=VERTEX_POINT('',#6259);
#1887=VERTEX_POINT('',#6260);
#1888=VERTEX_POINT('',#6310);
#1889=VERTEX_POINT('',#6311);
#1890=VERTEX_POINT('',#6358);
#1891=VERTEX_POINT('',#6359);
#1892=VERTEX_POINT('',#6406);
#1893=VERTEX_POINT('',#6407);
#1894=VERTEX_POINT('',#6457);
#1895=VERTEX_POINT('',#6458);
#1896=VERTEX_POINT('',#6508);
#1897=VERTEX_POINT('',#6509);
#1898=VERTEX_POINT('',#6556);
#1899=VERTEX_POINT('',#6557);
#1900=VERTEX_POINT('',#6607);
#1901=VERTEX_POINT('',#6608);
#1902=VERTEX_POINT('',#6610);
#1903=VERTEX_POINT('',#6624);
#1904=VERTEX_POINT('',#6646);
#1905=VERTEX_POINT('',#6647);
#1906=VERTEX_POINT('',#6649);
#1907=VERTEX_POINT('',#6654);
#1908=VERTEX_POINT('',#6667);
#1909=VERTEX_POINT('',#6668);
#1910=VERTEX_POINT('',#6718);
#1911=VERTEX_POINT('',#6719);
#1912=VERTEX_POINT('',#6769);
#1913=VERTEX_POINT('',#6770);
#1914=VERTEX_POINT('',#6817);
#1915=VERTEX_POINT('',#6818);
#1916=VERTEX_POINT('',#6865);
#1917=VERTEX_POINT('',#6866);
#1918=VERTEX_POINT('',#6916);
#1919=VERTEX_POINT('',#6917);
#1920=VERTEX_POINT('',#6967);
#1921=VERTEX_POINT('',#6968);
#1922=VERTEX_POINT('',#7015);
#1923=VERTEX_POINT('',#7016);
#1924=VERTEX_POINT('',#7066);
#1925=VERTEX_POINT('',#7067);
#1926=VERTEX_POINT('',#7069);
#1927=VERTEX_POINT('',#7083);
#1928=VERTEX_POINT('',#7105);
#1929=VERTEX_POINT('',#7106);
#1930=VERTEX_POINT('',#7108);
#1931=VERTEX_POINT('',#7113);
#1932=VERTEX_POINT('',#7126);
#1933=VERTEX_POINT('',#7127);
#1934=VERTEX_POINT('',#7177);
#1935=VERTEX_POINT('',#7178);
#1936=VERTEX_POINT('',#7228);
#1937=VERTEX_POINT('',#7229);
#1938=VERTEX_POINT('',#7276);
#1939=VERTEX_POINT('',#7277);
#1940=VERTEX_POINT('',#7324);
#1941=VERTEX_POINT('',#7325);
#1942=VERTEX_POINT('',#7375);
#1943=VERTEX_POINT('',#7376);
#1944=VERTEX_POINT('',#7426);
#1945=VERTEX_POINT('',#7427);
#1946=VERTEX_POINT('',#7474);
#1947=VERTEX_POINT('',#7475);
#1948=VERTEX_POINT('',#7525);
#1949=VERTEX_POINT('',#7526);
#1950=VERTEX_POINT('',#7528);
#1951=VERTEX_POINT('',#7542);
#1952=VERTEX_POINT('',#7564);
#1953=VERTEX_POINT('',#7565);
#1954=VERTEX_POINT('',#7567);
#1955=VERTEX_POINT('',#7572);
#1956=VERTEX_POINT('',#7585);
#1957=VERTEX_POINT('',#7586);
#1958=VERTEX_POINT('',#7636);
#1959=VERTEX_POINT('',#7637);
#1960=VERTEX_POINT('',#7687);
#1961=VERTEX_POINT('',#7688);
#1962=VERTEX_POINT('',#7735);
#1963=VERTEX_POINT('',#7736);
#1964=VERTEX_POINT('',#7783);
#1965=VERTEX_POINT('',#7784);
#1966=VERTEX_POINT('',#7834);
#1967=VERTEX_POINT('',#7835);
#1968=VERTEX_POINT('',#7885);
#1969=VERTEX_POINT('',#7886);
#1970=VERTEX_POINT('',#7933);
#1971=VERTEX_POINT('',#7934);
#1972=VERTEX_POINT('',#7984);
#1973=VERTEX_POINT('',#7985);
#1974=VERTEX_POINT('',#7987);
#1975=VERTEX_POINT('',#8001);
#1976=VERTEX_POINT('',#8023);
#1977=VERTEX_POINT('',#8024);
#1978=VERTEX_POINT('',#8026);
#1979=VERTEX_POINT('',#8035);
#1980=VERTEX_POINT('',#8047);
#1981=VERTEX_POINT('',#8048);
#1982=VERTEX_POINT('',#8071);
#1983=VERTEX_POINT('',#8072);
#1984=VERTEX_POINT('',#8096);
#1985=VERTEX_POINT('',#8097);
#1986=VERTEX_POINT('',#8120);
#1987=VERTEX_POINT('',#8121);
#1988=VERTEX_POINT('',#8145);
#1989=VERTEX_POINT('',#8146);
#1990=VERTEX_POINT('',#8169);
#1991=VERTEX_POINT('',#8170);
#1992=VERTEX_POINT('',#8194);
#1993=VERTEX_POINT('',#8195);
#1994=VERTEX_POINT('',#8219);
#1995=VERTEX_POINT('',#8220);
#1996=VERTEX_POINT('',#8243);
#1997=VERTEX_POINT('',#8244);
#1998=VERTEX_POINT('',#8246);
#1999=VERTEX_POINT('',#8252);
#2000=VERTEX_POINT('',#8260);
#2001=VERTEX_POINT('',#8261);
#2002=VERTEX_POINT('',#8263);
#2003=VERTEX_POINT('',#8272);
#2004=VERTEX_POINT('',#8284);
#2005=VERTEX_POINT('',#8285);
#2006=VERTEX_POINT('',#8308);
#2007=VERTEX_POINT('',#8309);
#2008=VERTEX_POINT('',#8333);
#2009=VERTEX_POINT('',#8334);
#2010=VERTEX_POINT('',#8357);
#2011=VERTEX_POINT('',#8358);
#2012=VERTEX_POINT('',#8382);
#2013=VERTEX_POINT('',#8383);
#2014=VERTEX_POINT('',#8406);
#2015=VERTEX_POINT('',#8407);
#2016=VERTEX_POINT('',#8431);
#2017=VERTEX_POINT('',#8432);
#2018=VERTEX_POINT('',#8456);
#2019=VERTEX_POINT('',#8457);
#2020=VERTEX_POINT('',#8480);
#2021=VERTEX_POINT('',#8481);
#2022=VERTEX_POINT('',#8483);
#2023=VERTEX_POINT('',#8489);
#2024=VERTEX_POINT('',#8497);
#2025=VERTEX_POINT('',#8498);
#2026=VERTEX_POINT('',#8500);
#2027=VERTEX_POINT('',#8509);
#2028=VERTEX_POINT('',#8521);
#2029=VERTEX_POINT('',#8522);
#2030=VERTEX_POINT('',#8545);
#2031=VERTEX_POINT('',#8546);
#2032=VERTEX_POINT('',#8570);
#2033=VERTEX_POINT('',#8571);
#2034=VERTEX_POINT('',#8594);
#2035=VERTEX_POINT('',#8595);
#2036=VERTEX_POINT('',#8619);
#2037=VERTEX_POINT('',#8620);
#2038=VERTEX_POINT('',#8643);
#2039=VERTEX_POINT('',#8644);
#2040=VERTEX_POINT('',#8668);
#2041=VERTEX_POINT('',#8669);
#2042=VERTEX_POINT('',#8693);
#2043=VERTEX_POINT('',#8694);
#2044=VERTEX_POINT('',#8717);
#2045=VERTEX_POINT('',#8718);
#2046=VERTEX_POINT('',#8720);
#2047=VERTEX_POINT('',#8726);
#2048=VERTEX_POINT('',#8734);
#2049=VERTEX_POINT('',#8735);
#2050=VERTEX_POINT('',#8737);
#2051=VERTEX_POINT('',#8746);
#2052=VERTEX_POINT('',#8758);
#2053=VERTEX_POINT('',#8759);
#2054=VERTEX_POINT('',#8782);
#2055=VERTEX_POINT('',#8783);
#2056=VERTEX_POINT('',#8807);
#2057=VERTEX_POINT('',#8808);
#2058=VERTEX_POINT('',#8831);
#2059=VERTEX_POINT('',#8832);
#2060=VERTEX_POINT('',#8856);
#2061=VERTEX_POINT('',#8857);
#2062=VERTEX_POINT('',#8880);
#2063=VERTEX_POINT('',#8881);
#2064=VERTEX_POINT('',#8905);
#2065=VERTEX_POINT('',#8906);
#2066=VERTEX_POINT('',#8930);
#2067=VERTEX_POINT('',#8931);
#2068=VERTEX_POINT('',#8954);
#2069=VERTEX_POINT('',#8955);
#2070=VERTEX_POINT('',#8957);
#2071=VERTEX_POINT('',#8963);
#2072=VERTEX_POINT('',#9966);
#2073=VERTEX_POINT('',#9967);
#2074=VERTEX_POINT('',#9969);
#2075=VERTEX_POINT('',#9971);
#2076=VERTEX_POINT('',#12964);
#2077=VERTEX_POINT('',#12965);
#2078=VERTEX_POINT('',#12970);
#2079=VERTEX_POINT('',#12974);
#2080=VERTEX_POINT('',#12982);
#2081=VERTEX_POINT('',#12983);
#2082=VERTEX_POINT('',#12985);
#2083=VERTEX_POINT('',#12987);
#2084=VERTEX_POINT('',#12991);
#2085=VERTEX_POINT('',#12993);
#2086=VERTEX_POINT('',#12997);
#2087=VERTEX_POINT('',#12999);
#2088=VERTEX_POINT('',#13009);
#2089=VERTEX_POINT('',#13011);
#2090=VERTEX_POINT('',#13015);
#2091=VERTEX_POINT('',#13017);
#2092=VERTEX_POINT('',#13024);
#2093=VERTEX_POINT('',#13026);
#2094=VERTEX_POINT('',#13030);
#2095=VERTEX_POINT('',#13032);
#2096=VERTEX_POINT('',#13039);
#2097=VERTEX_POINT('',#13041);
#2098=VERTEX_POINT('',#13045);
#2099=VERTEX_POINT('',#13048);
#2100=VERTEX_POINT('',#13051);
#2101=VERTEX_POINT('',#13055);
#2102=VERTEX_POINT('',#13057);
#2103=VERTEX_POINT('',#13060);
#2104=VERTEX_POINT('',#13069);
#2105=VERTEX_POINT('',#13070);
#2106=VERTEX_POINT('',#13072);
#2107=VERTEX_POINT('',#13074);
#2108=VERTEX_POINT('',#13078);
#2109=VERTEX_POINT('',#13079);
#2110=VERTEX_POINT('',#13081);
#2111=VERTEX_POINT('',#13083);
#2112=VERTEX_POINT('',#13096);
#2113=VERTEX_POINT('',#13098);
#2114=VERTEX_POINT('',#13102);
#2115=VERTEX_POINT('',#13104);
#2116=VERTEX_POINT('',#13111);
#2117=VERTEX_POINT('',#13113);
#2118=VERTEX_POINT('',#13117);
#2119=VERTEX_POINT('',#13119);
#2120=VERTEX_POINT('',#13126);
#2121=VERTEX_POINT('',#13128);
#2122=VERTEX_POINT('',#13132);
#2123=VERTEX_POINT('',#13134);
#2124=EDGE_CURVE('',#1752,#1753,#1648,.T.);
#2125=EDGE_CURVE('',#1753,#1754,#1124,.T.);
#2126=EDGE_CURVE('',#1754,#1755,#1649,.T.);
#2127=EDGE_CURVE('',#1755,#1752,#1125,.T.);
#2128=EDGE_CURVE('',#1756,#1753,#1126,.T.);
#2129=EDGE_CURVE('',#1757,#1756,#1127,.T.);
#2130=EDGE_CURVE('',#1757,#1754,#1128,.T.);
#2131=EDGE_CURVE('',#1752,#1758,#1129,.T.);
#2132=EDGE_CURVE('',#1759,#1758,#1650,.T.);
#2133=EDGE_CURVE('',#1759,#1760,#1130,.T.);
#2134=EDGE_CURVE('',#1761,#1760,#1651,.T.);
#2135=EDGE_CURVE('',#1761,#1762,#1131,.T.);
#2136=EDGE_CURVE('',#1756,#1762,#1652,.T.);
#2137=EDGE_CURVE('',#1763,#1764,#1132,.T.);
#2138=EDGE_CURVE('',#1765,#1764,#1653,.T.);
#2139=EDGE_CURVE('',#1765,#1766,#1133,.T.);
#2140=EDGE_CURVE('',#1767,#1766,#1654,.T.);
#2141=EDGE_CURVE('',#1767,#1768,#1134,.T.);
#2142=EDGE_CURVE('',#1769,#1768,#1655,.T.);
#2143=EDGE_CURVE('',#1769,#1770,#1135,.T.);
#2144=EDGE_CURVE('',#1763,#1770,#1656,.T.);
#2145=EDGE_CURVE('',#1758,#1771,#1136,.T.);
#2146=EDGE_CURVE('',#1771,#1772,#1657,.T.);
#2147=EDGE_CURVE('',#1772,#1759,#1137,.T.);
#2148=EDGE_CURVE('',#1772,#1773,#1138,.T.);
#2149=EDGE_CURVE('',#1760,#1773,#1139,.T.);
#2150=EDGE_CURVE('',#1773,#1774,#1658,.T.);
#2151=EDGE_CURVE('',#1774,#1761,#1140,.T.);
#2152=EDGE_CURVE('',#1762,#1775,#1141,.T.);
#2153=EDGE_CURVE('',#1775,#1757,#1659,.T.);
#2154=EDGE_CURVE('',#1776,#1777,#1660,.T.);
#2155=EDGE_CURVE('',#1777,#1765,#1142,.T.);
#2156=EDGE_CURVE('',#1764,#1776,#1143,.T.);
#2157=EDGE_CURVE('',#1777,#1778,#1144,.T.);
#2158=EDGE_CURVE('',#1766,#1778,#1145,.T.);
#2159=EDGE_CURVE('',#1778,#1779,#1661,.T.);
#2160=EDGE_CURVE('',#1779,#1767,#1146,.T.);
#2161=EDGE_CURVE('',#1779,#1780,#1147,.T.);
#2162=EDGE_CURVE('',#1768,#1780,#1148,.T.);
#2163=EDGE_CURVE('',#1780,#1781,#1662,.T.);
#2164=EDGE_CURVE('',#1781,#1769,#1149,.T.);
#2165=EDGE_CURVE('',#1781,#1782,#1150,.T.);
#2166=EDGE_CURVE('',#1770,#1782,#1151,.T.);
#2167=EDGE_CURVE('',#1782,#1783,#1663,.T.);
#2168=EDGE_CURVE('',#1783,#1763,#1152,.T.);
#2169=EDGE_CURVE('',#1783,#1776,#1153,.T.);
#2170=EDGE_CURVE('',#1774,#1775,#1154,.T.);
#2171=EDGE_CURVE('',#1755,#1771,#1155,.T.);
#2172=EDGE_CURVE('',#1784,#1785,#1664,.T.);
#2173=EDGE_CURVE('',#1785,#1786,#1156,.T.);
#2174=EDGE_CURVE('',#1786,#1787,#1665,.T.);
#2175=EDGE_CURVE('',#1787,#1784,#1157,.T.);
#2176=EDGE_CURVE('',#1788,#1785,#1158,.T.);
#2177=EDGE_CURVE('',#1789,#1788,#1159,.T.);
#2178=EDGE_CURVE('',#1789,#1786,#1160,.T.);
#2179=EDGE_CURVE('',#1784,#1790,#1161,.T.);
#2180=EDGE_CURVE('',#1791,#1790,#1666,.T.);
#2181=EDGE_CURVE('',#1791,#1792,#1162,.T.);
#2182=EDGE_CURVE('',#1793,#1792,#1667,.T.);
#2183=EDGE_CURVE('',#1793,#1794,#1163,.T.);
#2184=EDGE_CURVE('',#1788,#1794,#1668,.T.);
#2185=EDGE_CURVE('',#1795,#1796,#1164,.T.);
#2186=EDGE_CURVE('',#1797,#1796,#1669,.T.);
#2187=EDGE_CURVE('',#1797,#1798,#1165,.T.);
#2188=EDGE_CURVE('',#1799,#1798,#1670,.T.);
#2189=EDGE_CURVE('',#1799,#1800,#1166,.T.);
#2190=EDGE_CURVE('',#1801,#1800,#1671,.T.);
#2191=EDGE_CURVE('',#1801,#1802,#1167,.T.);
#2192=EDGE_CURVE('',#1795,#1802,#1672,.T.);
#2193=EDGE_CURVE('',#1790,#1803,#1168,.T.);
#2194=EDGE_CURVE('',#1803,#1804,#1673,.T.);
#2195=EDGE_CURVE('',#1804,#1791,#1169,.T.);
#2196=EDGE_CURVE('',#1804,#1805,#1170,.T.);
#2197=EDGE_CURVE('',#1792,#1805,#1171,.T.);
#2198=EDGE_CURVE('',#1805,#1806,#1674,.T.);
#2199=EDGE_CURVE('',#1806,#1793,#1172,.T.);
#2200=EDGE_CURVE('',#1794,#1807,#1173,.T.);
#2201=EDGE_CURVE('',#1807,#1789,#1675,.T.);
#2202=EDGE_CURVE('',#1808,#1809,#1676,.T.);
#2203=EDGE_CURVE('',#1809,#1797,#1174,.T.);
#2204=EDGE_CURVE('',#1796,#1808,#1175,.T.);
#2205=EDGE_CURVE('',#1809,#1810,#1176,.T.);
#2206=EDGE_CURVE('',#1798,#1810,#1177,.T.);
#2207=EDGE_CURVE('',#1810,#1811,#1677,.T.);
#2208=EDGE_CURVE('',#1811,#1799,#1178,.T.);
#2209=EDGE_CURVE('',#1811,#1812,#1179,.T.);
#2210=EDGE_CURVE('',#1800,#1812,#1180,.T.);
#2211=EDGE_CURVE('',#1812,#1813,#1678,.T.);
#2212=EDGE_CURVE('',#1813,#1801,#1181,.T.);
#2213=EDGE_CURVE('',#1813,#1814,#1182,.T.);
#2214=EDGE_CURVE('',#1802,#1814,#1183,.T.);
#2215=EDGE_CURVE('',#1814,#1815,#1679,.T.);
#2216=EDGE_CURVE('',#1815,#1795,#1184,.T.);
#2217=EDGE_CURVE('',#1815,#1808,#1185,.T.);
#2218=EDGE_CURVE('',#1806,#1807,#1186,.T.);
#2219=EDGE_CURVE('',#1787,#1803,#1187,.T.);
#2220=EDGE_CURVE('',#1816,#1816,#1680,.T.);
#2221=EDGE_CURVE('',#1816,#1817,#1188,.T.);
#2222=EDGE_CURVE('',#1817,#1817,#1681,.T.);
#2223=EDGE_CURVE('',#1818,#1818,#1682,.T.);
#2224=EDGE_CURVE('',#1818,#1819,#1189,.T.);
#2225=EDGE_CURVE('',#1819,#1819,#1683,.T.);
#2226=EDGE_CURVE('',#1820,#1820,#1684,.T.);
#2227=EDGE_CURVE('',#1820,#1821,#1190,.T.);
#2228=EDGE_CURVE('',#1821,#1821,#1685,.T.);
#2229=EDGE_CURVE('',#1822,#1822,#1686,.T.);
#2230=EDGE_CURVE('',#1822,#1823,#1191,.T.);
#2231=EDGE_CURVE('',#1823,#1823,#1687,.T.);
#2232=EDGE_CURVE('',#1824,#1825,#1192,.F.);
#2233=EDGE_CURVE('',#1825,#1826,#1193,.T.);
#2234=EDGE_CURVE('',#1827,#1826,#1194,.F.);
#2235=EDGE_CURVE('',#1824,#1827,#1195,.F.);
#2236=EDGE_CURVE('',#1828,#1824,#1196,.F.);
#2237=EDGE_CURVE('',#1829,#1827,#1197,.F.);
#2238=EDGE_CURVE('',#1828,#1829,#1198,.T.);
#2239=EDGE_CURVE('',#1830,#1828,#1199,.F.);
#2240=EDGE_CURVE('',#1831,#1829,#1200,.F.);
#2241=EDGE_CURVE('',#1830,#1831,#1201,.F.);
#2242=EDGE_CURVE('',#1825,#1830,#1202,.T.);
#2243=EDGE_CURVE('',#1826,#1831,#1203,.T.);
#2244=EDGE_CURVE('',#1832,#1832,#1688,.T.);
#2245=EDGE_CURVE('',#1832,#1833,#1204,.T.);
#2246=EDGE_CURVE('',#1833,#1833,#1689,.T.);
#2247=EDGE_CURVE('',#1834,#1834,#1690,.T.);
#2248=EDGE_CURVE('',#1834,#1835,#1205,.T.);
#2249=EDGE_CURVE('',#1835,#1835,#1691,.T.);
#2250=EDGE_CURVE('',#1836,#1836,#1692,.T.);
#2251=EDGE_CURVE('',#1836,#1837,#1206,.T.);
#2252=EDGE_CURVE('',#1837,#1837,#1693,.T.);
#2253=EDGE_CURVE('',#1838,#1838,#1694,.T.);
#2254=EDGE_CURVE('',#1838,#1839,#1207,.T.);
#2255=EDGE_CURVE('',#1839,#1839,#1695,.T.);
#2256=EDGE_CURVE('',#1840,#1841,#1208,.F.);
#2257=EDGE_CURVE('',#1841,#1842,#1209,.T.);
#2258=EDGE_CURVE('',#1843,#1842,#1210,.F.);
#2259=EDGE_CURVE('',#1840,#1843,#1211,.T.);
#2260=EDGE_CURVE('',#1844,#1840,#1212,.F.);
#2261=EDGE_CURVE('',#1845,#1843,#1213,.F.);
#2262=EDGE_CURVE('',#1844,#1845,#1214,.T.);
#2263=EDGE_CURVE('',#1846,#1844,#1215,.F.);
#2264=EDGE_CURVE('',#1847,#1845,#1216,.F.);
#2265=EDGE_CURVE('',#1846,#1847,#1217,.F.);
#2266=EDGE_CURVE('',#1841,#1846,#1218,.T.);
#2267=EDGE_CURVE('',#1842,#1847,#1219,.T.);
#2268=EDGE_CURVE('',#1848,#1849,#1220,.T.);
#2269=EDGE_CURVE('',#1849,#1850,#1221,.T.);
#2270=EDGE_CURVE('',#1851,#1850,#1222,.T.);
#2271=EDGE_CURVE('',#1848,#1851,#1223,.T.);
#2272=EDGE_CURVE('',#1852,#1848,#1224,.T.);
#2273=EDGE_CURVE('',#1853,#1851,#1225,.T.);
#2274=EDGE_CURVE('',#1852,#1853,#1226,.T.);
#2275=EDGE_CURVE('',#1854,#1852,#1227,.T.);
#2276=EDGE_CURVE('',#1855,#1853,#1228,.T.);
#2277=EDGE_CURVE('',#1854,#1855,#1229,.T.);
#2278=EDGE_CURVE('',#1849,#1854,#1230,.T.);
#2279=EDGE_CURVE('',#1850,#1855,#1231,.T.);
#2280=EDGE_CURVE('',#1856,#1857,#1232,.T.);
#2281=EDGE_CURVE('',#1857,#1858,#1233,.T.);
#2282=EDGE_CURVE('',#1859,#1858,#1234,.T.);
#2283=EDGE_CURVE('',#1856,#1859,#1235,.T.);
#2284=EDGE_CURVE('',#1860,#1856,#1236,.T.);
#2285=EDGE_CURVE('',#1861,#1859,#1237,.T.);
#2286=EDGE_CURVE('',#1860,#1861,#1238,.T.);
#2287=EDGE_CURVE('',#1862,#1860,#1239,.T.);
#2288=EDGE_CURVE('',#1863,#1861,#1240,.T.);
#2289=EDGE_CURVE('',#1862,#1863,#1241,.T.);
#2290=EDGE_CURVE('',#1857,#1862,#1242,.T.);
#2291=EDGE_CURVE('',#1858,#1863,#1243,.T.);
#2292=EDGE_CURVE('',#1864,#1864,#1696,.T.);
#2293=EDGE_CURVE('',#1864,#1865,#1244,.T.);
#2294=EDGE_CURVE('',#1865,#1865,#1697,.T.);
#2295=EDGE_CURVE('',#1866,#1866,#1698,.T.);
#2296=EDGE_CURVE('',#1866,#1867,#1245,.T.);
#2297=EDGE_CURVE('',#1867,#1867,#1699,.T.);
#2298=EDGE_CURVE('',#1868,#1868,#1700,.T.);
#2299=EDGE_CURVE('',#1868,#1869,#1246,.T.);
#2300=EDGE_CURVE('',#1869,#1869,#1701,.T.);
#2301=EDGE_CURVE('',#1870,#1870,#1702,.T.);
#2302=EDGE_CURVE('',#1870,#1871,#1247,.T.);
#2303=EDGE_CURVE('',#1871,#1871,#1703,.T.);
#2304=EDGE_CURVE('',#1872,#1873,#1248,.T.);
#2305=EDGE_CURVE('',#1873,#1874,#1249,.T.);
#2306=EDGE_CURVE('',#1875,#1874,#1250,.T.);
#2307=EDGE_CURVE('',#1872,#1875,#1251,.T.);
#2308=EDGE_CURVE('',#1876,#1872,#1252,.T.);
#2309=EDGE_CURVE('',#1877,#1875,#1253,.T.);
#2310=EDGE_CURVE('',#1876,#1877,#1254,.T.);
#2311=EDGE_CURVE('',#1878,#1876,#1255,.T.);
#2312=EDGE_CURVE('',#1879,#1877,#1256,.T.);
#2313=EDGE_CURVE('',#1878,#1879,#1257,.T.);
#2314=EDGE_CURVE('',#1873,#1878,#1258,.T.);
#2315=EDGE_CURVE('',#1874,#1879,#1259,.T.);
#2316=EDGE_CURVE('',#1880,#1881,#1260,.T.);
#2317=EDGE_CURVE('',#1881,#1882,#247,.T.);
#2318=EDGE_CURVE('',#1883,#1882,#1704,.F.);
#2319=EDGE_CURVE('',#1883,#1880,#248,.T.);
#2320=EDGE_CURVE('',#1884,#1885,#1261,.T.);
#2321=EDGE_CURVE('',#1885,#1881,#249,.T.);
#2322=EDGE_CURVE('',#1880,#1884,#250,.T.);
#2323=EDGE_CURVE('',#1886,#1887,#1262,.T.);
#2324=EDGE_CURVE('',#1887,#1885,#251,.T.);
#2325=EDGE_CURVE('',#1884,#1886,#252,.T.);
#2326=EDGE_CURVE('',#1888,#1889,#1263,.T.);
#2327=EDGE_CURVE('',#1889,#1887,#253,.T.);
#2328=EDGE_CURVE('',#1886,#1888,#254,.T.);
#2329=EDGE_CURVE('',#1890,#1891,#1264,.T.);
#2330=EDGE_CURVE('',#1891,#1889,#255,.T.);
#2331=EDGE_CURVE('',#1888,#1890,#256,.T.);
#2332=EDGE_CURVE('',#1892,#1893,#1265,.T.);
#2333=EDGE_CURVE('',#1893,#1891,#257,.T.);
#2334=EDGE_CURVE('',#1890,#1892,#258,.T.);
#2335=EDGE_CURVE('',#1894,#1895,#1266,.T.);
#2336=EDGE_CURVE('',#1895,#1893,#259,.T.);
#2337=EDGE_CURVE('',#1892,#1894,#260,.T.);
#2338=EDGE_CURVE('',#1896,#1897,#1267,.T.);
#2339=EDGE_CURVE('',#1897,#1895,#261,.T.);
#2340=EDGE_CURVE('',#1894,#1896,#262,.T.);
#2341=EDGE_CURVE('',#1898,#1899,#1268,.T.);
#2342=EDGE_CURVE('',#1899,#1897,#263,.T.);
#2343=EDGE_CURVE('',#1896,#1898,#264,.T.);
#2344=EDGE_CURVE('',#1900,#1901,#1269,.T.);
#2345=EDGE_CURVE('',#1900,#1902,#265,.T.);
#2346=EDGE_CURVE('',#1903,#1902,#1705,.T.);
#2347=EDGE_CURVE('',#1903,#1901,#266,.T.);
#2348=EDGE_CURVE('',#1904,#1905,#1270,.T.);
#2349=EDGE_CURVE('',#1905,#1906,#267,.T.);
#2350=EDGE_CURVE('',#1907,#1906,#1706,.F.);
#2351=EDGE_CURVE('',#1907,#1904,#268,.T.);
#2352=EDGE_CURVE('',#1908,#1909,#1271,.T.);
#2353=EDGE_CURVE('',#1909,#1905,#269,.T.);
#2354=EDGE_CURVE('',#1904,#1908,#270,.T.);
#2355=EDGE_CURVE('',#1910,#1911,#1272,.T.);
#2356=EDGE_CURVE('',#1911,#1909,#271,.T.);
#2357=EDGE_CURVE('',#1908,#1910,#272,.T.);
#2358=EDGE_CURVE('',#1912,#1913,#1273,.T.);
#2359=EDGE_CURVE('',#1913,#1911,#273,.T.);
#2360=EDGE_CURVE('',#1910,#1912,#274,.T.);
#2361=EDGE_CURVE('',#1914,#1915,#1274,.T.);
#2362=EDGE_CURVE('',#1915,#1913,#275,.T.);
#2363=EDGE_CURVE('',#1912,#1914,#276,.T.);
#2364=EDGE_CURVE('',#1916,#1917,#1275,.T.);
#2365=EDGE_CURVE('',#1917,#1915,#277,.T.);
#2366=EDGE_CURVE('',#1914,#1916,#278,.T.);
#2367=EDGE_CURVE('',#1918,#1919,#1276,.T.);
#2368=EDGE_CURVE('',#1919,#1917,#279,.T.);
#2369=EDGE_CURVE('',#1916,#1918,#280,.T.);
#2370=EDGE_CURVE('',#1920,#1921,#1277,.T.);
#2371=EDGE_CURVE('',#1921,#1919,#281,.T.);
#2372=EDGE_CURVE('',#1918,#1920,#282,.T.);
#2373=EDGE_CURVE('',#1922,#1923,#1278,.T.);
#2374=EDGE_CURVE('',#1923,#1921,#283,.T.);
#2375=EDGE_CURVE('',#1920,#1922,#284,.T.);
#2376=EDGE_CURVE('',#1924,#1925,#1279,.T.);
#2377=EDGE_CURVE('',#1924,#1926,#285,.T.);
#2378=EDGE_CURVE('',#1927,#1926,#1707,.T.);
#2379=EDGE_CURVE('',#1927,#1925,#286,.T.);
#2380=EDGE_CURVE('',#1928,#1929,#1280,.T.);
#2381=EDGE_CURVE('',#1929,#1930,#287,.T.);
#2382=EDGE_CURVE('',#1931,#1930,#1708,.F.);
#2383=EDGE_CURVE('',#1931,#1928,#288,.T.);
#2384=EDGE_CURVE('',#1932,#1933,#1281,.T.);
#2385=EDGE_CURVE('',#1933,#1929,#289,.T.);
#2386=EDGE_CURVE('',#1928,#1932,#290,.T.);
#2387=EDGE_CURVE('',#1934,#1935,#1282,.T.);
#2388=EDGE_CURVE('',#1935,#1933,#291,.T.);
#2389=EDGE_CURVE('',#1932,#1934,#292,.T.);
#2390=EDGE_CURVE('',#1936,#1937,#1283,.T.);
#2391=EDGE_CURVE('',#1937,#1935,#293,.T.);
#2392=EDGE_CURVE('',#1934,#1936,#294,.T.);
#2393=EDGE_CURVE('',#1938,#1939,#1284,.T.);
#2394=EDGE_CURVE('',#1939,#1937,#295,.T.);
#2395=EDGE_CURVE('',#1936,#1938,#296,.T.);
#2396=EDGE_CURVE('',#1940,#1941,#1285,.T.);
#2397=EDGE_CURVE('',#1941,#1939,#297,.T.);
#2398=EDGE_CURVE('',#1938,#1940,#298,.T.);
#2399=EDGE_CURVE('',#1942,#1943,#1286,.T.);
#2400=EDGE_CURVE('',#1943,#1941,#299,.T.);
#2401=EDGE_CURVE('',#1940,#1942,#300,.T.);
#2402=EDGE_CURVE('',#1944,#1945,#1287,.T.);
#2403=EDGE_CURVE('',#1945,#1943,#301,.T.);
#2404=EDGE_CURVE('',#1942,#1944,#302,.T.);
#2405=EDGE_CURVE('',#1946,#1947,#1288,.T.);
#2406=EDGE_CURVE('',#1947,#1945,#303,.T.);
#2407=EDGE_CURVE('',#1944,#1946,#304,.T.);
#2408=EDGE_CURVE('',#1948,#1949,#1289,.T.);
#2409=EDGE_CURVE('',#1948,#1950,#305,.T.);
#2410=EDGE_CURVE('',#1951,#1950,#1709,.T.);
#2411=EDGE_CURVE('',#1951,#1949,#306,.T.);
#2412=EDGE_CURVE('',#1952,#1953,#1290,.T.);
#2413=EDGE_CURVE('',#1953,#1954,#307,.T.);
#2414=EDGE_CURVE('',#1955,#1954,#1710,.F.);
#2415=EDGE_CURVE('',#1955,#1952,#308,.T.);
#2416=EDGE_CURVE('',#1956,#1957,#1291,.T.);
#2417=EDGE_CURVE('',#1957,#1953,#309,.T.);
#2418=EDGE_CURVE('',#1952,#1956,#310,.T.);
#2419=EDGE_CURVE('',#1958,#1959,#1292,.T.);
#2420=EDGE_CURVE('',#1959,#1957,#311,.T.);
#2421=EDGE_CURVE('',#1956,#1958,#312,.T.);
#2422=EDGE_CURVE('',#1960,#1961,#1293,.T.);
#2423=EDGE_CURVE('',#1961,#1959,#313,.T.);
#2424=EDGE_CURVE('',#1958,#1960,#314,.T.);
#2425=EDGE_CURVE('',#1962,#1963,#1294,.T.);
#2426=EDGE_CURVE('',#1963,#1961,#315,.T.);
#2427=EDGE_CURVE('',#1960,#1962,#316,.T.);
#2428=EDGE_CURVE('',#1964,#1965,#1295,.T.);
#2429=EDGE_CURVE('',#1965,#1963,#317,.T.);
#2430=EDGE_CURVE('',#1962,#1964,#318,.T.);
#2431=EDGE_CURVE('',#1966,#1967,#1296,.T.);
#2432=EDGE_CURVE('',#1967,#1965,#319,.T.);
#2433=EDGE_CURVE('',#1964,#1966,#320,.T.);
#2434=EDGE_CURVE('',#1968,#1969,#1297,.T.);
#2435=EDGE_CURVE('',#1969,#1967,#321,.T.);
#2436=EDGE_CURVE('',#1966,#1968,#322,.T.);
#2437=EDGE_CURVE('',#1970,#1971,#1298,.T.);
#2438=EDGE_CURVE('',#1971,#1969,#323,.T.);
#2439=EDGE_CURVE('',#1968,#1970,#324,.T.);
#2440=EDGE_CURVE('',#1972,#1973,#1299,.T.);
#2441=EDGE_CURVE('',#1972,#1974,#325,.T.);
#2442=EDGE_CURVE('',#1975,#1974,#1711,.T.);
#2443=EDGE_CURVE('',#1975,#1973,#326,.T.);
#2444=EDGE_CURVE('',#1976,#1977,#1300,.T.);
#2445=EDGE_CURVE('',#1977,#1978,#327,.T.);
#2446=EDGE_CURVE('',#1979,#1978,#1712,.T.);
#2447=EDGE_CURVE('',#1976,#1979,#328,.T.);
#2448=EDGE_CURVE('',#1980,#1981,#1301,.T.);
#2449=EDGE_CURVE('',#1981,#1977,#329,.T.);
#2450=EDGE_CURVE('',#1980,#1976,#330,.T.);
#2451=EDGE_CURVE('',#1982,#1983,#1302,.T.);
#2452=EDGE_CURVE('',#1983,#1981,#331,.T.);
#2453=EDGE_CURVE('',#1982,#1980,#332,.T.);
#2454=EDGE_CURVE('',#1984,#1985,#1303,.T.);
#2455=EDGE_CURVE('',#1985,#1983,#333,.T.);
#2456=EDGE_CURVE('',#1984,#1982,#334,.T.);
#2457=EDGE_CURVE('',#1986,#1987,#1304,.T.);
#2458=EDGE_CURVE('',#1987,#1985,#335,.T.);
#2459=EDGE_CURVE('',#1986,#1984,#336,.T.);
#2460=EDGE_CURVE('',#1988,#1989,#1305,.T.);
#2461=EDGE_CURVE('',#1989,#1987,#337,.T.);
#2462=EDGE_CURVE('',#1988,#1986,#338,.T.);
#2463=EDGE_CURVE('',#1990,#1991,#1306,.T.);
#2464=EDGE_CURVE('',#1991,#1989,#339,.T.);
#2465=EDGE_CURVE('',#1990,#1988,#340,.T.);
#2466=EDGE_CURVE('',#1992,#1993,#1307,.T.);
#2467=EDGE_CURVE('',#1993,#1991,#341,.T.);
#2468=EDGE_CURVE('',#1992,#1990,#342,.T.);
#2469=EDGE_CURVE('',#1994,#1995,#1308,.T.);
#2470=EDGE_CURVE('',#1995,#1993,#343,.T.);
#2471=EDGE_CURVE('',#1994,#1992,#344,.T.);
#2472=EDGE_CURVE('',#1996,#1997,#1309,.T.);
#2473=EDGE_CURVE('',#1998,#1996,#345,.T.);
#2474=EDGE_CURVE('',#1999,#1998,#1713,.T.);
#2475=EDGE_CURVE('',#1999,#1997,#346,.T.);
#2476=EDGE_CURVE('',#2000,#2001,#1310,.T.);
#2477=EDGE_CURVE('',#2001,#2002,#347,.T.);
#2478=EDGE_CURVE('',#2003,#2002,#1714,.T.);
#2479=EDGE_CURVE('',#2000,#2003,#348,.T.);
#2480=EDGE_CURVE('',#2004,#2005,#1311,.T.);
#2481=EDGE_CURVE('',#2005,#2001,#349,.T.);
#2482=EDGE_CURVE('',#2004,#2000,#350,.T.);
#2483=EDGE_CURVE('',#2006,#2007,#1312,.T.);
#2484=EDGE_CURVE('',#2007,#2005,#351,.T.);
#2485=EDGE_CURVE('',#2006,#2004,#352,.T.);
#2486=EDGE_CURVE('',#2008,#2009,#1313,.T.);
#2487=EDGE_CURVE('',#2009,#2007,#353,.T.);
#2488=EDGE_CURVE('',#2008,#2006,#354,.T.);
#2489=EDGE_CURVE('',#2010,#2011,#1314,.T.);
#2490=EDGE_CURVE('',#2011,#2009,#355,.T.);
#2491=EDGE_CURVE('',#2010,#2008,#356,.T.);
#2492=EDGE_CURVE('',#2012,#2013,#1315,.T.);
#2493=EDGE_CURVE('',#2013,#2011,#357,.T.);
#2494=EDGE_CURVE('',#2012,#2010,#358,.T.);
#2495=EDGE_CURVE('',#2014,#2015,#1316,.T.);
#2496=EDGE_CURVE('',#2015,#2013,#359,.T.);
#2497=EDGE_CURVE('',#2014,#2012,#360,.T.);
#2498=EDGE_CURVE('',#2016,#2017,#1317,.T.);
#2499=EDGE_CURVE('',#2017,#2015,#361,.T.);
#2500=EDGE_CURVE('',#2016,#2014,#362,.T.);
#2501=EDGE_CURVE('',#2018,#2019,#1318,.T.);
#2502=EDGE_CURVE('',#2019,#2017,#363,.T.);
#2503=EDGE_CURVE('',#2018,#2016,#364,.T.);
#2504=EDGE_CURVE('',#2020,#2021,#1319,.T.);
#2505=EDGE_CURVE('',#2022,#2020,#365,.T.);
#2506=EDGE_CURVE('',#2023,#2022,#1715,.T.);
#2507=EDGE_CURVE('',#2023,#2021,#366,.T.);
#2508=EDGE_CURVE('',#2024,#2025,#1320,.T.);
#2509=EDGE_CURVE('',#2025,#2026,#367,.T.);
#2510=EDGE_CURVE('',#2027,#2026,#1716,.T.);
#2511=EDGE_CURVE('',#2024,#2027,#368,.T.);
#2512=EDGE_CURVE('',#2028,#2029,#1321,.T.);
#2513=EDGE_CURVE('',#2029,#2025,#369,.T.);
#2514=EDGE_CURVE('',#2028,#2024,#370,.T.);
#2515=EDGE_CURVE('',#2030,#2031,#1322,.T.);
#2516=EDGE_CURVE('',#2031,#2029,#371,.T.);
#2517=EDGE_CURVE('',#2030,#2028,#372,.T.);
#2518=EDGE_CURVE('',#2032,#2033,#1323,.T.);
#2519=EDGE_CURVE('',#2033,#2031,#373,.T.);
#2520=EDGE_CURVE('',#2032,#2030,#374,.T.);
#2521=EDGE_CURVE('',#2034,#2035,#1324,.T.);
#2522=EDGE_CURVE('',#2035,#2033,#375,.T.);
#2523=EDGE_CURVE('',#2034,#2032,#376,.T.);
#2524=EDGE_CURVE('',#2036,#2037,#1325,.T.);
#2525=EDGE_CURVE('',#2037,#2035,#377,.T.);
#2526=EDGE_CURVE('',#2036,#2034,#378,.T.);
#2527=EDGE_CURVE('',#2038,#2039,#1326,.T.);
#2528=EDGE_CURVE('',#2039,#2037,#379,.T.);
#2529=EDGE_CURVE('',#2038,#2036,#380,.T.);
#2530=EDGE_CURVE('',#2040,#2041,#1327,.T.);
#2531=EDGE_CURVE('',#2041,#2039,#381,.T.);
#2532=EDGE_CURVE('',#2040,#2038,#382,.T.);
#2533=EDGE_CURVE('',#2042,#2043,#1328,.T.);
#2534=EDGE_CURVE('',#2043,#2041,#383,.T.);
#2535=EDGE_CURVE('',#2042,#2040,#384,.T.);
#2536=EDGE_CURVE('',#2044,#2045,#1329,.T.);
#2537=EDGE_CURVE('',#2046,#2044,#385,.T.);
#2538=EDGE_CURVE('',#2047,#2046,#1717,.T.);
#2539=EDGE_CURVE('',#2047,#2045,#386,.T.);
#2540=EDGE_CURVE('',#2048,#2049,#1330,.T.);
#2541=EDGE_CURVE('',#2049,#2050,#387,.T.);
#2542=EDGE_CURVE('',#2051,#2050,#1718,.T.);
#2543=EDGE_CURVE('',#2048,#2051,#388,.T.);
#2544=EDGE_CURVE('',#2052,#2053,#1331,.T.);
#2545=EDGE_CURVE('',#2053,#2049,#389,.T.);
#2546=EDGE_CURVE('',#2052,#2048,#390,.T.);
#2547=EDGE_CURVE('',#2054,#2055,#1332,.T.);
#2548=EDGE_CURVE('',#2055,#2053,#391,.T.);
#2549=EDGE_CURVE('',#2054,#2052,#392,.T.);
#2550=EDGE_CURVE('',#2056,#2057,#1333,.T.);
#2551=EDGE_CURVE('',#2057,#2055,#393,.T.);
#2552=EDGE_CURVE('',#2056,#2054,#394,.T.);
#2553=EDGE_CURVE('',#2058,#2059,#1334,.T.);
#2554=EDGE_CURVE('',#2059,#2057,#395,.T.);
#2555=EDGE_CURVE('',#2058,#2056,#396,.T.);
#2556=EDGE_CURVE('',#2060,#2061,#1335,.T.);
#2557=EDGE_CURVE('',#2061,#2059,#397,.T.);
#2558=EDGE_CURVE('',#2060,#2058,#398,.T.);
#2559=EDGE_CURVE('',#2062,#2063,#1336,.T.);
#2560=EDGE_CURVE('',#2063,#2061,#399,.T.);
#2561=EDGE_CURVE('',#2062,#2060,#400,.T.);
#2562=EDGE_CURVE('',#2064,#2065,#1337,.T.);
#2563=EDGE_CURVE('',#2065,#2063,#401,.T.);
#2564=EDGE_CURVE('',#2064,#2062,#402,.T.);
#2565=EDGE_CURVE('',#2066,#2067,#1338,.T.);
#2566=EDGE_CURVE('',#2067,#2065,#403,.T.);
#2567=EDGE_CURVE('',#2066,#2064,#404,.T.);
#2568=EDGE_CURVE('',#2068,#2069,#1339,.T.);
#2569=EDGE_CURVE('',#2070,#2068,#405,.T.);
#2570=EDGE_CURVE('',#2071,#2070,#1719,.T.);
#2571=EDGE_CURVE('',#2071,#2069,#406,.T.);
#2572=EDGE_CURVE('',#2069,#2067,#407,.T.);
#2573=EDGE_CURVE('',#2068,#2066,#408,.T.);
#2574=EDGE_CURVE('',#2050,#1931,#409,.T.);
#2575=EDGE_CURVE('',#1950,#2071,#410,.T.);
#2576=EDGE_CURVE('',#1946,#1948,#411,.T.);
#2577=EDGE_CURVE('',#1930,#2051,#412,.T.);
#2578=EDGE_CURVE('',#1949,#1947,#413,.T.);
#2579=EDGE_CURVE('',#2070,#1951,#414,.T.);
#2580=EDGE_CURVE('',#2072,#2073,#1340,.T.);
#2581=EDGE_CURVE('',#2073,#2074,#1341,.T.);
#2582=EDGE_CURVE('',#2074,#2075,#1342,.T.);
#2583=EDGE_CURVE('',#2075,#2072,#1343,.T.);
#2584=EDGE_CURVE('',#1974,#2047,#415,.T.);
#2585=EDGE_CURVE('',#2046,#1975,#416,.T.);
#2586=EDGE_CURVE('',#1926,#2023,#417,.T.);
#2587=EDGE_CURVE('',#2022,#1927,#418,.T.);
#2588=EDGE_CURVE('',#1902,#1999,#419,.T.);
#2589=EDGE_CURVE('',#1998,#1903,#420,.T.);
#2590=EDGE_CURVE('',#2045,#2043,#421,.T.);
#2591=EDGE_CURVE('',#2044,#2042,#422,.T.);
#2592=EDGE_CURVE('',#2026,#1955,#423,.T.);
#2593=EDGE_CURVE('',#1970,#1972,#424,.T.);
#2594=EDGE_CURVE('',#1954,#2027,#425,.T.);
#2595=EDGE_CURVE('',#1973,#1971,#426,.T.);
#2596=EDGE_CURVE('',#2021,#2019,#427,.T.);
#2597=EDGE_CURVE('',#2020,#2018,#428,.T.);
#2598=EDGE_CURVE('',#2002,#1907,#429,.T.);
#2599=EDGE_CURVE('',#1922,#1924,#430,.T.);
#2600=EDGE_CURVE('',#1906,#2003,#431,.T.);
#2601=EDGE_CURVE('',#1925,#1923,#432,.T.);
#2602=EDGE_CURVE('',#1997,#1995,#433,.T.);
#2603=EDGE_CURVE('',#1996,#1994,#434,.T.);
#2604=EDGE_CURVE('',#1978,#1883,#435,.T.);
#2605=EDGE_CURVE('',#1898,#1900,#436,.T.);
#2606=EDGE_CURVE('',#1882,#1979,#437,.T.);
#2607=EDGE_CURVE('',#1901,#1899,#438,.T.);
#2608=EDGE_CURVE('',#2076,#2077,#1344,.T.);
#2609=EDGE_CURVE('',#2077,#2072,#1345,.T.);
#2610=EDGE_CURVE('',#2076,#2075,#1346,.T.);
#2611=EDGE_CURVE('',#2078,#2076,#1347,.T.);
#2612=EDGE_CURVE('',#2078,#2074,#1348,.T.);
#2613=EDGE_CURVE('',#2079,#2078,#1349,.T.);
#2614=EDGE_CURVE('',#2079,#2073,#1350,.T.);
#2615=EDGE_CURVE('',#2077,#2079,#1351,.T.);
#2616=EDGE_CURVE('',#2080,#2081,#1352,.T.);
#2617=EDGE_CURVE('',#2081,#2082,#1353,.T.);
#2618=EDGE_CURVE('',#2083,#2082,#1354,.T.);
#2619=EDGE_CURVE('',#2080,#2083,#1355,.T.);
#2620=EDGE_CURVE('',#2084,#2080,#1356,.T.);
#2621=EDGE_CURVE('',#2085,#2083,#1357,.T.);
#2622=EDGE_CURVE('',#2084,#2085,#1358,.T.);
#2623=EDGE_CURVE('',#2086,#2084,#1359,.T.);
#2624=EDGE_CURVE('',#2087,#2085,#1360,.T.);
#2625=EDGE_CURVE('',#2086,#2087,#1361,.T.);
#2626=EDGE_CURVE('',#2081,#2086,#1362,.T.);
#2627=EDGE_CURVE('',#2082,#2087,#1363,.T.);
#2628=EDGE_CURVE('',#2088,#2088,#1720,.T.);
#2629=EDGE_CURVE('',#2088,#2089,#1364,.T.);
#2630=EDGE_CURVE('',#2089,#2089,#1721,.T.);
#2631=EDGE_CURVE('',#2090,#2090,#1722,.T.);
#2632=EDGE_CURVE('',#2090,#2091,#1365,.T.);
#2633=EDGE_CURVE('',#2091,#2091,#1723,.T.);
#2634=EDGE_CURVE('',#2092,#2092,#1724,.T.);
#2635=EDGE_CURVE('',#2092,#2093,#1366,.T.);
#2636=EDGE_CURVE('',#2093,#2093,#1725,.T.);
#2637=EDGE_CURVE('',#2094,#2094,#1726,.T.);
#2638=EDGE_CURVE('',#2094,#2095,#1367,.T.);
#2639=EDGE_CURVE('',#2095,#2095,#1727,.T.);
#2640=EDGE_CURVE('',#2096,#2096,#1728,.T.);
#2641=EDGE_CURVE('',#2096,#2097,#1368,.T.);
#2642=EDGE_CURVE('',#2097,#2097,#1729,.T.);
#2643=EDGE_CURVE('',#2098,#2098,#1730,.T.);
#2644=EDGE_CURVE('',#2099,#2099,#1731,.T.);
#2645=EDGE_CURVE('',#2100,#2100,#1732,.T.);
#2646=EDGE_CURVE('',#2100,#2099,#1369,.T.);
#2647=EDGE_CURVE('',#2101,#2101,#1733,.T.);
#2648=EDGE_CURVE('',#2102,#2102,#1734,.T.);
#2649=EDGE_CURVE('',#2101,#2103,#1370,.T.);
#2650=EDGE_CURVE('',#2103,#2103,#1735,.T.);
#2651=EDGE_CURVE('',#2098,#2102,#1371,.T.);
#2652=EDGE_CURVE('',#2104,#2105,#1372,.T.);
#2653=EDGE_CURVE('',#2106,#2104,#1373,.T.);
#2654=EDGE_CURVE('',#2107,#2106,#1374,.T.);
#2655=EDGE_CURVE('',#2105,#2107,#1375,.T.);
#2656=EDGE_CURVE('',#2108,#2109,#1376,.T.);
#2657=EDGE_CURVE('',#2110,#2108,#1377,.T.);
#2658=EDGE_CURVE('',#2111,#2110,#1378,.T.);
#2659=EDGE_CURVE('',#2109,#2111,#1379,.T.);
#2660=EDGE_CURVE('',#2106,#2111,#1736,.T.);
#2661=EDGE_CURVE('',#2109,#2104,#1737,.T.);
#2662=EDGE_CURVE('',#2108,#2105,#1738,.T.);
#2663=EDGE_CURVE('',#2107,#2110,#1739,.T.);
#2664=EDGE_CURVE('',#2112,#2112,#1740,.T.);
#2665=EDGE_CURVE('',#2112,#2113,#1380,.T.);
#2666=EDGE_CURVE('',#2113,#2113,#1741,.T.);
#2667=EDGE_CURVE('',#2114,#2114,#1742,.T.);
#2668=EDGE_CURVE('',#2114,#2115,#1381,.T.);
#2669=EDGE_CURVE('',#2115,#2115,#1743,.T.);
#2670=EDGE_CURVE('',#2116,#2116,#1744,.T.);
#2671=EDGE_CURVE('',#2116,#2117,#1382,.T.);
#2672=EDGE_CURVE('',#2117,#2117,#1745,.T.);
#2673=EDGE_CURVE('',#2118,#2118,#1746,.T.);
#2674=EDGE_CURVE('',#2118,#2119,#1383,.T.);
#2675=EDGE_CURVE('',#2119,#2119,#1747,.T.);
#2676=EDGE_CURVE('',#2120,#2120,#1748,.T.);
#2677=EDGE_CURVE('',#2120,#2121,#1384,.T.);
#2678=EDGE_CURVE('',#2121,#2121,#1749,.T.);
#2679=EDGE_CURVE('',#2122,#2122,#1750,.T.);
#2680=EDGE_CURVE('',#2122,#2123,#1385,.T.);
#2681=EDGE_CURVE('',#2123,#2123,#1751,.T.);
#2682=ORIENTED_EDGE('',*,*,#2124,.T.);
#2683=ORIENTED_EDGE('',*,*,#2125,.T.);
#2684=ORIENTED_EDGE('',*,*,#2126,.T.);
#2685=ORIENTED_EDGE('',*,*,#2127,.T.);
#2686=ORIENTED_EDGE('',*,*,#2125,.F.);
#2687=ORIENTED_EDGE('',*,*,#2128,.F.);
#2688=ORIENTED_EDGE('',*,*,#2129,.F.);
#2689=ORIENTED_EDGE('',*,*,#2130,.T.);
#2690=ORIENTED_EDGE('',*,*,#2124,.F.);
#2691=ORIENTED_EDGE('',*,*,#2131,.T.);
#2692=ORIENTED_EDGE('',*,*,#2132,.F.);
#2693=ORIENTED_EDGE('',*,*,#2133,.T.);
#2694=ORIENTED_EDGE('',*,*,#2134,.F.);
#2695=ORIENTED_EDGE('',*,*,#2135,.T.);
#2696=ORIENTED_EDGE('',*,*,#2136,.F.);
#2697=ORIENTED_EDGE('',*,*,#2128,.T.);
#2698=ORIENTED_EDGE('',*,*,#2137,.T.);
#2699=ORIENTED_EDGE('',*,*,#2138,.F.);
#2700=ORIENTED_EDGE('',*,*,#2139,.T.);
#2701=ORIENTED_EDGE('',*,*,#2140,.F.);
#2702=ORIENTED_EDGE('',*,*,#2141,.T.);
#2703=ORIENTED_EDGE('',*,*,#2142,.F.);
#2704=ORIENTED_EDGE('',*,*,#2143,.T.);
#2705=ORIENTED_EDGE('',*,*,#2144,.F.);
#2706=ORIENTED_EDGE('',*,*,#2132,.T.);
#2707=ORIENTED_EDGE('',*,*,#2145,.T.);
#2708=ORIENTED_EDGE('',*,*,#2146,.T.);
#2709=ORIENTED_EDGE('',*,*,#2147,.T.);
#2710=ORIENTED_EDGE('',*,*,#2147,.F.);
#2711=ORIENTED_EDGE('',*,*,#2148,.T.);
#2712=ORIENTED_EDGE('',*,*,#2149,.F.);
#2713=ORIENTED_EDGE('',*,*,#2133,.F.);
#2714=ORIENTED_EDGE('',*,*,#2134,.T.);
#2715=ORIENTED_EDGE('',*,*,#2149,.T.);
#2716=ORIENTED_EDGE('',*,*,#2150,.T.);
#2717=ORIENTED_EDGE('',*,*,#2151,.T.);
#2718=ORIENTED_EDGE('',*,*,#2136,.T.);
#2719=ORIENTED_EDGE('',*,*,#2152,.T.);
#2720=ORIENTED_EDGE('',*,*,#2153,.T.);
#2721=ORIENTED_EDGE('',*,*,#2129,.T.);
#2722=ORIENTED_EDGE('',*,*,#2154,.T.);
#2723=ORIENTED_EDGE('',*,*,#2155,.T.);
#2724=ORIENTED_EDGE('',*,*,#2138,.T.);
#2725=ORIENTED_EDGE('',*,*,#2156,.T.);
#2726=ORIENTED_EDGE('',*,*,#2155,.F.);
#2727=ORIENTED_EDGE('',*,*,#2157,.T.);
#2728=ORIENTED_EDGE('',*,*,#2158,.F.);
#2729=ORIENTED_EDGE('',*,*,#2139,.F.);
#2730=ORIENTED_EDGE('',*,*,#2159,.T.);
#2731=ORIENTED_EDGE('',*,*,#2160,.T.);
#2732=ORIENTED_EDGE('',*,*,#2140,.T.);
#2733=ORIENTED_EDGE('',*,*,#2158,.T.);
#2734=ORIENTED_EDGE('',*,*,#2160,.F.);
#2735=ORIENTED_EDGE('',*,*,#2161,.T.);
#2736=ORIENTED_EDGE('',*,*,#2162,.F.);
#2737=ORIENTED_EDGE('',*,*,#2141,.F.);
#2738=ORIENTED_EDGE('',*,*,#2163,.T.);
#2739=ORIENTED_EDGE('',*,*,#2164,.T.);
#2740=ORIENTED_EDGE('',*,*,#2142,.T.);
#2741=ORIENTED_EDGE('',*,*,#2162,.T.);
#2742=ORIENTED_EDGE('',*,*,#2164,.F.);
#2743=ORIENTED_EDGE('',*,*,#2165,.T.);
#2744=ORIENTED_EDGE('',*,*,#2166,.F.);
#2745=ORIENTED_EDGE('',*,*,#2143,.F.);
#2746=ORIENTED_EDGE('',*,*,#2167,.T.);
#2747=ORIENTED_EDGE('',*,*,#2168,.T.);
#2748=ORIENTED_EDGE('',*,*,#2144,.T.);
#2749=ORIENTED_EDGE('',*,*,#2166,.T.);
#2750=ORIENTED_EDGE('',*,*,#2156,.F.);
#2751=ORIENTED_EDGE('',*,*,#2137,.F.);
#2752=ORIENTED_EDGE('',*,*,#2168,.F.);
#2753=ORIENTED_EDGE('',*,*,#2169,.T.);
#2754=ORIENTED_EDGE('',*,*,#2151,.F.);
#2755=ORIENTED_EDGE('',*,*,#2170,.T.);
#2756=ORIENTED_EDGE('',*,*,#2152,.F.);
#2757=ORIENTED_EDGE('',*,*,#2135,.F.);
#2758=ORIENTED_EDGE('',*,*,#2127,.F.);
#2759=ORIENTED_EDGE('',*,*,#2171,.T.);
#2760=ORIENTED_EDGE('',*,*,#2145,.F.);
#2761=ORIENTED_EDGE('',*,*,#2131,.F.);
#2762=ORIENTED_EDGE('',*,*,#2126,.F.);
#2763=ORIENTED_EDGE('',*,*,#2130,.F.);
#2764=ORIENTED_EDGE('',*,*,#2153,.F.);
#2765=ORIENTED_EDGE('',*,*,#2170,.F.);
#2766=ORIENTED_EDGE('',*,*,#2150,.F.);
#2767=ORIENTED_EDGE('',*,*,#2148,.F.);
#2768=ORIENTED_EDGE('',*,*,#2146,.F.);
#2769=ORIENTED_EDGE('',*,*,#2171,.F.);
#2770=ORIENTED_EDGE('',*,*,#2167,.F.);
#2771=ORIENTED_EDGE('',*,*,#2165,.F.);
#2772=ORIENTED_EDGE('',*,*,#2163,.F.);
#2773=ORIENTED_EDGE('',*,*,#2161,.F.);
#2774=ORIENTED_EDGE('',*,*,#2159,.F.);
#2775=ORIENTED_EDGE('',*,*,#2157,.F.);
#2776=ORIENTED_EDGE('',*,*,#2154,.F.);
#2777=ORIENTED_EDGE('',*,*,#2169,.F.);
#2778=ORIENTED_EDGE('',*,*,#2172,.T.);
#2779=ORIENTED_EDGE('',*,*,#2173,.T.);
#2780=ORIENTED_EDGE('',*,*,#2174,.T.);
#2781=ORIENTED_EDGE('',*,*,#2175,.T.);
#2782=ORIENTED_EDGE('',*,*,#2173,.F.);
#2783=ORIENTED_EDGE('',*,*,#2176,.F.);
#2784=ORIENTED_EDGE('',*,*,#2177,.F.);
#2785=ORIENTED_EDGE('',*,*,#2178,.T.);
#2786=ORIENTED_EDGE('',*,*,#2172,.F.);
#2787=ORIENTED_EDGE('',*,*,#2179,.T.);
#2788=ORIENTED_EDGE('',*,*,#2180,.F.);
#2789=ORIENTED_EDGE('',*,*,#2181,.T.);
#2790=ORIENTED_EDGE('',*,*,#2182,.F.);
#2791=ORIENTED_EDGE('',*,*,#2183,.T.);
#2792=ORIENTED_EDGE('',*,*,#2184,.F.);
#2793=ORIENTED_EDGE('',*,*,#2176,.T.);
#2794=ORIENTED_EDGE('',*,*,#2185,.T.);
#2795=ORIENTED_EDGE('',*,*,#2186,.F.);
#2796=ORIENTED_EDGE('',*,*,#2187,.T.);
#2797=ORIENTED_EDGE('',*,*,#2188,.F.);
#2798=ORIENTED_EDGE('',*,*,#2189,.T.);
#2799=ORIENTED_EDGE('',*,*,#2190,.F.);
#2800=ORIENTED_EDGE('',*,*,#2191,.T.);
#2801=ORIENTED_EDGE('',*,*,#2192,.F.);
#2802=ORIENTED_EDGE('',*,*,#2180,.T.);
#2803=ORIENTED_EDGE('',*,*,#2193,.T.);
#2804=ORIENTED_EDGE('',*,*,#2194,.T.);
#2805=ORIENTED_EDGE('',*,*,#2195,.T.);
#2806=ORIENTED_EDGE('',*,*,#2195,.F.);
#2807=ORIENTED_EDGE('',*,*,#2196,.T.);
#2808=ORIENTED_EDGE('',*,*,#2197,.F.);
#2809=ORIENTED_EDGE('',*,*,#2181,.F.);
#2810=ORIENTED_EDGE('',*,*,#2182,.T.);
#2811=ORIENTED_EDGE('',*,*,#2197,.T.);
#2812=ORIENTED_EDGE('',*,*,#2198,.T.);
#2813=ORIENTED_EDGE('',*,*,#2199,.T.);
#2814=ORIENTED_EDGE('',*,*,#2184,.T.);
#2815=ORIENTED_EDGE('',*,*,#2200,.T.);
#2816=ORIENTED_EDGE('',*,*,#2201,.T.);
#2817=ORIENTED_EDGE('',*,*,#2177,.T.);
#2818=ORIENTED_EDGE('',*,*,#2202,.T.);
#2819=ORIENTED_EDGE('',*,*,#2203,.T.);
#2820=ORIENTED_EDGE('',*,*,#2186,.T.);
#2821=ORIENTED_EDGE('',*,*,#2204,.T.);
#2822=ORIENTED_EDGE('',*,*,#2203,.F.);
#2823=ORIENTED_EDGE('',*,*,#2205,.T.);
#2824=ORIENTED_EDGE('',*,*,#2206,.F.);
#2825=ORIENTED_EDGE('',*,*,#2187,.F.);
#2826=ORIENTED_EDGE('',*,*,#2207,.T.);
#2827=ORIENTED_EDGE('',*,*,#2208,.T.);
#2828=ORIENTED_EDGE('',*,*,#2188,.T.);
#2829=ORIENTED_EDGE('',*,*,#2206,.T.);
#2830=ORIENTED_EDGE('',*,*,#2208,.F.);
#2831=ORIENTED_EDGE('',*,*,#2209,.T.);
#2832=ORIENTED_EDGE('',*,*,#2210,.F.);
#2833=ORIENTED_EDGE('',*,*,#2189,.F.);
#2834=ORIENTED_EDGE('',*,*,#2211,.T.);
#2835=ORIENTED_EDGE('',*,*,#2212,.T.);
#2836=ORIENTED_EDGE('',*,*,#2190,.T.);
#2837=ORIENTED_EDGE('',*,*,#2210,.T.);
#2838=ORIENTED_EDGE('',*,*,#2212,.F.);
#2839=ORIENTED_EDGE('',*,*,#2213,.T.);
#2840=ORIENTED_EDGE('',*,*,#2214,.F.);
#2841=ORIENTED_EDGE('',*,*,#2191,.F.);
#2842=ORIENTED_EDGE('',*,*,#2215,.T.);
#2843=ORIENTED_EDGE('',*,*,#2216,.T.);
#2844=ORIENTED_EDGE('',*,*,#2192,.T.);
#2845=ORIENTED_EDGE('',*,*,#2214,.T.);
#2846=ORIENTED_EDGE('',*,*,#2204,.F.);
#2847=ORIENTED_EDGE('',*,*,#2185,.F.);
#2848=ORIENTED_EDGE('',*,*,#2216,.F.);
#2849=ORIENTED_EDGE('',*,*,#2217,.T.);
#2850=ORIENTED_EDGE('',*,*,#2199,.F.);
#2851=ORIENTED_EDGE('',*,*,#2218,.T.);
#2852=ORIENTED_EDGE('',*,*,#2200,.F.);
#2853=ORIENTED_EDGE('',*,*,#2183,.F.);
#2854=ORIENTED_EDGE('',*,*,#2175,.F.);
#2855=ORIENTED_EDGE('',*,*,#2219,.T.);
#2856=ORIENTED_EDGE('',*,*,#2193,.F.);
#2857=ORIENTED_EDGE('',*,*,#2179,.F.);
#2858=ORIENTED_EDGE('',*,*,#2174,.F.);
#2859=ORIENTED_EDGE('',*,*,#2178,.F.);
#2860=ORIENTED_EDGE('',*,*,#2201,.F.);
#2861=ORIENTED_EDGE('',*,*,#2218,.F.);
#2862=ORIENTED_EDGE('',*,*,#2198,.F.);
#2863=ORIENTED_EDGE('',*,*,#2196,.F.);
#2864=ORIENTED_EDGE('',*,*,#2194,.F.);
#2865=ORIENTED_EDGE('',*,*,#2219,.F.);
#2866=ORIENTED_EDGE('',*,*,#2215,.F.);
#2867=ORIENTED_EDGE('',*,*,#2213,.F.);
#2868=ORIENTED_EDGE('',*,*,#2211,.F.);
#2869=ORIENTED_EDGE('',*,*,#2209,.F.);
#2870=ORIENTED_EDGE('',*,*,#2207,.F.);
#2871=ORIENTED_EDGE('',*,*,#2205,.F.);
#2872=ORIENTED_EDGE('',*,*,#2202,.F.);
#2873=ORIENTED_EDGE('',*,*,#2217,.F.);
#2874=ORIENTED_EDGE('',*,*,#2220,.F.);
#2875=ORIENTED_EDGE('',*,*,#2221,.T.);
#2876=ORIENTED_EDGE('',*,*,#2222,.F.);
#2877=ORIENTED_EDGE('',*,*,#2221,.F.);
#2878=ORIENTED_EDGE('',*,*,#2223,.F.);
#2879=ORIENTED_EDGE('',*,*,#2224,.T.);
#2880=ORIENTED_EDGE('',*,*,#2225,.F.);
#2881=ORIENTED_EDGE('',*,*,#2224,.F.);
#2882=ORIENTED_EDGE('',*,*,#2226,.F.);
#2883=ORIENTED_EDGE('',*,*,#2227,.T.);
#2884=ORIENTED_EDGE('',*,*,#2228,.F.);
#2885=ORIENTED_EDGE('',*,*,#2227,.F.);
#2886=ORIENTED_EDGE('',*,*,#2229,.F.);
#2887=ORIENTED_EDGE('',*,*,#2230,.T.);
#2888=ORIENTED_EDGE('',*,*,#2231,.F.);
#2889=ORIENTED_EDGE('',*,*,#2230,.F.);
#2890=ORIENTED_EDGE('',*,*,#2232,.T.);
#2891=ORIENTED_EDGE('',*,*,#2233,.T.);
#2892=ORIENTED_EDGE('',*,*,#2234,.F.);
#2893=ORIENTED_EDGE('',*,*,#2235,.F.);
#2894=ORIENTED_EDGE('',*,*,#2236,.T.);
#2895=ORIENTED_EDGE('',*,*,#2235,.T.);
#2896=ORIENTED_EDGE('',*,*,#2237,.F.);
#2897=ORIENTED_EDGE('',*,*,#2238,.F.);
#2898=ORIENTED_EDGE('',*,*,#2239,.T.);
#2899=ORIENTED_EDGE('',*,*,#2238,.T.);
#2900=ORIENTED_EDGE('',*,*,#2240,.F.);
#2901=ORIENTED_EDGE('',*,*,#2241,.F.);
#2902=ORIENTED_EDGE('',*,*,#2242,.T.);
#2903=ORIENTED_EDGE('',*,*,#2241,.T.);
#2904=ORIENTED_EDGE('',*,*,#2243,.F.);
#2905=ORIENTED_EDGE('',*,*,#2233,.F.);
#2906=ORIENTED_EDGE('',*,*,#2243,.T.);
#2907=ORIENTED_EDGE('',*,*,#2240,.T.);
#2908=ORIENTED_EDGE('',*,*,#2237,.T.);
#2909=ORIENTED_EDGE('',*,*,#2234,.T.);
#2910=ORIENTED_EDGE('',*,*,#2220,.T.);
#2911=ORIENTED_EDGE('',*,*,#2223,.T.);
#2912=ORIENTED_EDGE('',*,*,#2226,.T.);
#2913=ORIENTED_EDGE('',*,*,#2229,.T.);
#2914=ORIENTED_EDGE('',*,*,#2242,.F.);
#2915=ORIENTED_EDGE('',*,*,#2232,.F.);
#2916=ORIENTED_EDGE('',*,*,#2236,.F.);
#2917=ORIENTED_EDGE('',*,*,#2239,.F.);
#2918=ORIENTED_EDGE('',*,*,#2222,.T.);
#2919=ORIENTED_EDGE('',*,*,#2225,.T.);
#2920=ORIENTED_EDGE('',*,*,#2228,.T.);
#2921=ORIENTED_EDGE('',*,*,#2231,.T.);
#2922=ORIENTED_EDGE('',*,*,#2244,.F.);
#2923=ORIENTED_EDGE('',*,*,#2245,.T.);
#2924=ORIENTED_EDGE('',*,*,#2246,.F.);
#2925=ORIENTED_EDGE('',*,*,#2245,.F.);
#2926=ORIENTED_EDGE('',*,*,#2247,.F.);
#2927=ORIENTED_EDGE('',*,*,#2248,.T.);
#2928=ORIENTED_EDGE('',*,*,#2249,.F.);
#2929=ORIENTED_EDGE('',*,*,#2248,.F.);
#2930=ORIENTED_EDGE('',*,*,#2250,.F.);
#2931=ORIENTED_EDGE('',*,*,#2251,.T.);
#2932=ORIENTED_EDGE('',*,*,#2252,.F.);
#2933=ORIENTED_EDGE('',*,*,#2251,.F.);
#2934=ORIENTED_EDGE('',*,*,#2253,.F.);
#2935=ORIENTED_EDGE('',*,*,#2254,.T.);
#2936=ORIENTED_EDGE('',*,*,#2255,.F.);
#2937=ORIENTED_EDGE('',*,*,#2254,.F.);
#2938=ORIENTED_EDGE('',*,*,#2256,.T.);
#2939=ORIENTED_EDGE('',*,*,#2257,.T.);
#2940=ORIENTED_EDGE('',*,*,#2258,.F.);
#2941=ORIENTED_EDGE('',*,*,#2259,.F.);
#2942=ORIENTED_EDGE('',*,*,#2260,.T.);
#2943=ORIENTED_EDGE('',*,*,#2259,.T.);
#2944=ORIENTED_EDGE('',*,*,#2261,.F.);
#2945=ORIENTED_EDGE('',*,*,#2262,.F.);
#2946=ORIENTED_EDGE('',*,*,#2263,.T.);
#2947=ORIENTED_EDGE('',*,*,#2262,.T.);
#2948=ORIENTED_EDGE('',*,*,#2264,.F.);
#2949=ORIENTED_EDGE('',*,*,#2265,.F.);
#2950=ORIENTED_EDGE('',*,*,#2266,.T.);
#2951=ORIENTED_EDGE('',*,*,#2265,.T.);
#2952=ORIENTED_EDGE('',*,*,#2267,.F.);
#2953=ORIENTED_EDGE('',*,*,#2257,.F.);
#2954=ORIENTED_EDGE('',*,*,#2267,.T.);
#2955=ORIENTED_EDGE('',*,*,#2264,.T.);
#2956=ORIENTED_EDGE('',*,*,#2261,.T.);
#2957=ORIENTED_EDGE('',*,*,#2258,.T.);
#2958=ORIENTED_EDGE('',*,*,#2244,.T.);
#2959=ORIENTED_EDGE('',*,*,#2247,.T.);
#2960=ORIENTED_EDGE('',*,*,#2250,.T.);
#2961=ORIENTED_EDGE('',*,*,#2253,.T.);
#2962=ORIENTED_EDGE('',*,*,#2266,.F.);
#2963=ORIENTED_EDGE('',*,*,#2256,.F.);
#2964=ORIENTED_EDGE('',*,*,#2260,.F.);
#2965=ORIENTED_EDGE('',*,*,#2263,.F.);
#2966=ORIENTED_EDGE('',*,*,#2246,.T.);
#2967=ORIENTED_EDGE('',*,*,#2249,.T.);
#2968=ORIENTED_EDGE('',*,*,#2252,.T.);
#2969=ORIENTED_EDGE('',*,*,#2255,.T.);
#2970=ORIENTED_EDGE('',*,*,#2268,.T.);
#2971=ORIENTED_EDGE('',*,*,#2269,.T.);
#2972=ORIENTED_EDGE('',*,*,#2270,.F.);
#2973=ORIENTED_EDGE('',*,*,#2271,.F.);
#2974=ORIENTED_EDGE('',*,*,#2272,.T.);
#2975=ORIENTED_EDGE('',*,*,#2271,.T.);
#2976=ORIENTED_EDGE('',*,*,#2273,.F.);
#2977=ORIENTED_EDGE('',*,*,#2274,.F.);
#2978=ORIENTED_EDGE('',*,*,#2275,.T.);
#2979=ORIENTED_EDGE('',*,*,#2274,.T.);
#2980=ORIENTED_EDGE('',*,*,#2276,.F.);
#2981=ORIENTED_EDGE('',*,*,#2277,.F.);
#2982=ORIENTED_EDGE('',*,*,#2278,.T.);
#2983=ORIENTED_EDGE('',*,*,#2277,.T.);
#2984=ORIENTED_EDGE('',*,*,#2279,.F.);
#2985=ORIENTED_EDGE('',*,*,#2269,.F.);
#2986=ORIENTED_EDGE('',*,*,#2279,.T.);
#2987=ORIENTED_EDGE('',*,*,#2276,.T.);
#2988=ORIENTED_EDGE('',*,*,#2273,.T.);
#2989=ORIENTED_EDGE('',*,*,#2270,.T.);
#2990=ORIENTED_EDGE('',*,*,#2278,.F.);
#2991=ORIENTED_EDGE('',*,*,#2268,.F.);
#2992=ORIENTED_EDGE('',*,*,#2272,.F.);
#2993=ORIENTED_EDGE('',*,*,#2275,.F.);
#2994=ORIENTED_EDGE('',*,*,#2280,.T.);
#2995=ORIENTED_EDGE('',*,*,#2281,.T.);
#2996=ORIENTED_EDGE('',*,*,#2282,.F.);
#2997=ORIENTED_EDGE('',*,*,#2283,.F.);
#2998=ORIENTED_EDGE('',*,*,#2284,.T.);
#2999=ORIENTED_EDGE('',*,*,#2283,.T.);
#3000=ORIENTED_EDGE('',*,*,#2285,.F.);
#3001=ORIENTED_EDGE('',*,*,#2286,.F.);
#3002=ORIENTED_EDGE('',*,*,#2287,.T.);
#3003=ORIENTED_EDGE('',*,*,#2286,.T.);
#3004=ORIENTED_EDGE('',*,*,#2288,.F.);
#3005=ORIENTED_EDGE('',*,*,#2289,.F.);
#3006=ORIENTED_EDGE('',*,*,#2290,.T.);
#3007=ORIENTED_EDGE('',*,*,#2289,.T.);
#3008=ORIENTED_EDGE('',*,*,#2291,.F.);
#3009=ORIENTED_EDGE('',*,*,#2281,.F.);
#3010=ORIENTED_EDGE('',*,*,#2291,.T.);
#3011=ORIENTED_EDGE('',*,*,#2288,.T.);
#3012=ORIENTED_EDGE('',*,*,#2285,.T.);
#3013=ORIENTED_EDGE('',*,*,#2282,.T.);
#3014=ORIENTED_EDGE('',*,*,#2290,.F.);
#3015=ORIENTED_EDGE('',*,*,#2280,.F.);
#3016=ORIENTED_EDGE('',*,*,#2284,.F.);
#3017=ORIENTED_EDGE('',*,*,#2287,.F.);
#3018=ORIENTED_EDGE('',*,*,#2292,.F.);
#3019=ORIENTED_EDGE('',*,*,#2293,.T.);
#3020=ORIENTED_EDGE('',*,*,#2294,.F.);
#3021=ORIENTED_EDGE('',*,*,#2293,.F.);
#3022=ORIENTED_EDGE('',*,*,#2295,.F.);
#3023=ORIENTED_EDGE('',*,*,#2296,.T.);
#3024=ORIENTED_EDGE('',*,*,#2297,.F.);
#3025=ORIENTED_EDGE('',*,*,#2296,.F.);
#3026=ORIENTED_EDGE('',*,*,#2298,.F.);
#3027=ORIENTED_EDGE('',*,*,#2299,.T.);
#3028=ORIENTED_EDGE('',*,*,#2300,.F.);
#3029=ORIENTED_EDGE('',*,*,#2299,.F.);
#3030=ORIENTED_EDGE('',*,*,#2301,.F.);
#3031=ORIENTED_EDGE('',*,*,#2302,.T.);
#3032=ORIENTED_EDGE('',*,*,#2303,.F.);
#3033=ORIENTED_EDGE('',*,*,#2302,.F.);
#3034=ORIENTED_EDGE('',*,*,#2304,.T.);
#3035=ORIENTED_EDGE('',*,*,#2305,.T.);
#3036=ORIENTED_EDGE('',*,*,#2306,.F.);
#3037=ORIENTED_EDGE('',*,*,#2307,.F.);
#3038=ORIENTED_EDGE('',*,*,#2292,.T.);
#3039=ORIENTED_EDGE('',*,*,#2295,.T.);
#3040=ORIENTED_EDGE('',*,*,#2298,.T.);
#3041=ORIENTED_EDGE('',*,*,#2301,.T.);
#3042=ORIENTED_EDGE('',*,*,#2308,.T.);
#3043=ORIENTED_EDGE('',*,*,#2307,.T.);
#3044=ORIENTED_EDGE('',*,*,#2309,.F.);
#3045=ORIENTED_EDGE('',*,*,#2310,.F.);
#3046=ORIENTED_EDGE('',*,*,#2311,.T.);
#3047=ORIENTED_EDGE('',*,*,#2310,.T.);
#3048=ORIENTED_EDGE('',*,*,#2312,.F.);
#3049=ORIENTED_EDGE('',*,*,#2313,.F.);
#3050=ORIENTED_EDGE('',*,*,#2294,.T.);
#3051=ORIENTED_EDGE('',*,*,#2297,.T.);
#3052=ORIENTED_EDGE('',*,*,#2300,.T.);
#3053=ORIENTED_EDGE('',*,*,#2303,.T.);
#3054=ORIENTED_EDGE('',*,*,#2314,.T.);
#3055=ORIENTED_EDGE('',*,*,#2313,.T.);
#3056=ORIENTED_EDGE('',*,*,#2315,.F.);
#3057=ORIENTED_EDGE('',*,*,#2305,.F.);
#3058=ORIENTED_EDGE('',*,*,#2315,.T.);
#3059=ORIENTED_EDGE('',*,*,#2312,.T.);
#3060=ORIENTED_EDGE('',*,*,#2309,.T.);
#3061=ORIENTED_EDGE('',*,*,#2306,.T.);
#3062=ORIENTED_EDGE('',*,*,#2314,.F.);
#3063=ORIENTED_EDGE('',*,*,#2304,.F.);
#3064=ORIENTED_EDGE('',*,*,#2308,.F.);
#3065=ORIENTED_EDGE('',*,*,#2311,.F.);
#3066=ORIENTED_EDGE('',*,*,#2316,.T.);
#3067=ORIENTED_EDGE('',*,*,#2317,.T.);
#3068=ORIENTED_EDGE('',*,*,#2318,.F.);
#3069=ORIENTED_EDGE('',*,*,#2319,.T.);
#3070=ORIENTED_EDGE('',*,*,#2320,.T.);
#3071=ORIENTED_EDGE('',*,*,#2321,.T.);
#3072=ORIENTED_EDGE('',*,*,#2316,.F.);
#3073=ORIENTED_EDGE('',*,*,#2322,.T.);
#3074=ORIENTED_EDGE('',*,*,#2323,.T.);
#3075=ORIENTED_EDGE('',*,*,#2324,.T.);
#3076=ORIENTED_EDGE('',*,*,#2320,.F.);
#3077=ORIENTED_EDGE('',*,*,#2325,.T.);
#3078=ORIENTED_EDGE('',*,*,#2326,.T.);
#3079=ORIENTED_EDGE('',*,*,#2327,.T.);
#3080=ORIENTED_EDGE('',*,*,#2323,.F.);
#3081=ORIENTED_EDGE('',*,*,#2328,.T.);
#3082=ORIENTED_EDGE('',*,*,#2329,.T.);
#3083=ORIENTED_EDGE('',*,*,#2330,.T.);
#3084=ORIENTED_EDGE('',*,*,#2326,.F.);
#3085=ORIENTED_EDGE('',*,*,#2331,.T.);
#3086=ORIENTED_EDGE('',*,*,#2332,.T.);
#3087=ORIENTED_EDGE('',*,*,#2333,.T.);
#3088=ORIENTED_EDGE('',*,*,#2329,.F.);
#3089=ORIENTED_EDGE('',*,*,#2334,.T.);
#3090=ORIENTED_EDGE('',*,*,#2335,.T.);
#3091=ORIENTED_EDGE('',*,*,#2336,.T.);
#3092=ORIENTED_EDGE('',*,*,#2332,.F.);
#3093=ORIENTED_EDGE('',*,*,#2337,.T.);
#3094=ORIENTED_EDGE('',*,*,#2338,.T.);
#3095=ORIENTED_EDGE('',*,*,#2339,.T.);
#3096=ORIENTED_EDGE('',*,*,#2335,.F.);
#3097=ORIENTED_EDGE('',*,*,#2340,.T.);
#3098=ORIENTED_EDGE('',*,*,#2341,.T.);
#3099=ORIENTED_EDGE('',*,*,#2342,.T.);
#3100=ORIENTED_EDGE('',*,*,#2338,.F.);
#3101=ORIENTED_EDGE('',*,*,#2343,.T.);
#3102=ORIENTED_EDGE('',*,*,#2344,.F.);
#3103=ORIENTED_EDGE('',*,*,#2345,.T.);
#3104=ORIENTED_EDGE('',*,*,#2346,.F.);
#3105=ORIENTED_EDGE('',*,*,#2347,.T.);
#3106=ORIENTED_EDGE('',*,*,#2348,.T.);
#3107=ORIENTED_EDGE('',*,*,#2349,.T.);
#3108=ORIENTED_EDGE('',*,*,#2350,.F.);
#3109=ORIENTED_EDGE('',*,*,#2351,.T.);
#3110=ORIENTED_EDGE('',*,*,#2352,.T.);
#3111=ORIENTED_EDGE('',*,*,#2353,.T.);
#3112=ORIENTED_EDGE('',*,*,#2348,.F.);
#3113=ORIENTED_EDGE('',*,*,#2354,.T.);
#3114=ORIENTED_EDGE('',*,*,#2355,.T.);
#3115=ORIENTED_EDGE('',*,*,#2356,.T.);
#3116=ORIENTED_EDGE('',*,*,#2352,.F.);
#3117=ORIENTED_EDGE('',*,*,#2357,.T.);
#3118=ORIENTED_EDGE('',*,*,#2358,.T.);
#3119=ORIENTED_EDGE('',*,*,#2359,.T.);
#3120=ORIENTED_EDGE('',*,*,#2355,.F.);
#3121=ORIENTED_EDGE('',*,*,#2360,.T.);
#3122=ORIENTED_EDGE('',*,*,#2361,.T.);
#3123=ORIENTED_EDGE('',*,*,#2362,.T.);
#3124=ORIENTED_EDGE('',*,*,#2358,.F.);
#3125=ORIENTED_EDGE('',*,*,#2363,.T.);
#3126=ORIENTED_EDGE('',*,*,#2364,.T.);
#3127=ORIENTED_EDGE('',*,*,#2365,.T.);
#3128=ORIENTED_EDGE('',*,*,#2361,.F.);
#3129=ORIENTED_EDGE('',*,*,#2366,.T.);
#3130=ORIENTED_EDGE('',*,*,#2367,.T.);
#3131=ORIENTED_EDGE('',*,*,#2368,.T.);
#3132=ORIENTED_EDGE('',*,*,#2364,.F.);
#3133=ORIENTED_EDGE('',*,*,#2369,.T.);
#3134=ORIENTED_EDGE('',*,*,#2370,.T.);
#3135=ORIENTED_EDGE('',*,*,#2371,.T.);
#3136=ORIENTED_EDGE('',*,*,#2367,.F.);
#3137=ORIENTED_EDGE('',*,*,#2372,.T.);
#3138=ORIENTED_EDGE('',*,*,#2373,.T.);
#3139=ORIENTED_EDGE('',*,*,#2374,.T.);
#3140=ORIENTED_EDGE('',*,*,#2370,.F.);
#3141=ORIENTED_EDGE('',*,*,#2375,.T.);
#3142=ORIENTED_EDGE('',*,*,#2376,.F.);
#3143=ORIENTED_EDGE('',*,*,#2377,.T.);
#3144=ORIENTED_EDGE('',*,*,#2378,.F.);
#3145=ORIENTED_EDGE('',*,*,#2379,.T.);
#3146=ORIENTED_EDGE('',*,*,#2380,.T.);
#3147=ORIENTED_EDGE('',*,*,#2381,.T.);
#3148=ORIENTED_EDGE('',*,*,#2382,.F.);
#3149=ORIENTED_EDGE('',*,*,#2383,.T.);
#3150=ORIENTED_EDGE('',*,*,#2384,.T.);
#3151=ORIENTED_EDGE('',*,*,#2385,.T.);
#3152=ORIENTED_EDGE('',*,*,#2380,.F.);
#3153=ORIENTED_EDGE('',*,*,#2386,.T.);
#3154=ORIENTED_EDGE('',*,*,#2387,.T.);
#3155=ORIENTED_EDGE('',*,*,#2388,.T.);
#3156=ORIENTED_EDGE('',*,*,#2384,.F.);
#3157=ORIENTED_EDGE('',*,*,#2389,.T.);
#3158=ORIENTED_EDGE('',*,*,#2390,.T.);
#3159=ORIENTED_EDGE('',*,*,#2391,.T.);
#3160=ORIENTED_EDGE('',*,*,#2387,.F.);
#3161=ORIENTED_EDGE('',*,*,#2392,.T.);
#3162=ORIENTED_EDGE('',*,*,#2393,.T.);
#3163=ORIENTED_EDGE('',*,*,#2394,.T.);
#3164=ORIENTED_EDGE('',*,*,#2390,.F.);
#3165=ORIENTED_EDGE('',*,*,#2395,.T.);
#3166=ORIENTED_EDGE('',*,*,#2396,.T.);
#3167=ORIENTED_EDGE('',*,*,#2397,.T.);
#3168=ORIENTED_EDGE('',*,*,#2393,.F.);
#3169=ORIENTED_EDGE('',*,*,#2398,.T.);
#3170=ORIENTED_EDGE('',*,*,#2399,.T.);
#3171=ORIENTED_EDGE('',*,*,#2400,.T.);
#3172=ORIENTED_EDGE('',*,*,#2396,.F.);
#3173=ORIENTED_EDGE('',*,*,#2401,.T.);
#3174=ORIENTED_EDGE('',*,*,#2402,.T.);
#3175=ORIENTED_EDGE('',*,*,#2403,.T.);
#3176=ORIENTED_EDGE('',*,*,#2399,.F.);
#3177=ORIENTED_EDGE('',*,*,#2404,.T.);
#3178=ORIENTED_EDGE('',*,*,#2405,.T.);
#3179=ORIENTED_EDGE('',*,*,#2406,.T.);
#3180=ORIENTED_EDGE('',*,*,#2402,.F.);
#3181=ORIENTED_EDGE('',*,*,#2407,.T.);
#3182=ORIENTED_EDGE('',*,*,#2408,.F.);
#3183=ORIENTED_EDGE('',*,*,#2409,.T.);
#3184=ORIENTED_EDGE('',*,*,#2410,.F.);
#3185=ORIENTED_EDGE('',*,*,#2411,.T.);
#3186=ORIENTED_EDGE('',*,*,#2412,.T.);
#3187=ORIENTED_EDGE('',*,*,#2413,.T.);
#3188=ORIENTED_EDGE('',*,*,#2414,.F.);
#3189=ORIENTED_EDGE('',*,*,#2415,.T.);
#3190=ORIENTED_EDGE('',*,*,#2416,.T.);
#3191=ORIENTED_EDGE('',*,*,#2417,.T.);
#3192=ORIENTED_EDGE('',*,*,#2412,.F.);
#3193=ORIENTED_EDGE('',*,*,#2418,.T.);
#3194=ORIENTED_EDGE('',*,*,#2419,.T.);
#3195=ORIENTED_EDGE('',*,*,#2420,.T.);
#3196=ORIENTED_EDGE('',*,*,#2416,.F.);
#3197=ORIENTED_EDGE('',*,*,#2421,.T.);
#3198=ORIENTED_EDGE('',*,*,#2422,.T.);
#3199=ORIENTED_EDGE('',*,*,#2423,.T.);
#3200=ORIENTED_EDGE('',*,*,#2419,.F.);
#3201=ORIENTED_EDGE('',*,*,#2424,.T.);
#3202=ORIENTED_EDGE('',*,*,#2425,.T.);
#3203=ORIENTED_EDGE('',*,*,#2426,.T.);
#3204=ORIENTED_EDGE('',*,*,#2422,.F.);
#3205=ORIENTED_EDGE('',*,*,#2427,.T.);
#3206=ORIENTED_EDGE('',*,*,#2428,.T.);
#3207=ORIENTED_EDGE('',*,*,#2429,.T.);
#3208=ORIENTED_EDGE('',*,*,#2425,.F.);
#3209=ORIENTED_EDGE('',*,*,#2430,.T.);
#3210=ORIENTED_EDGE('',*,*,#2431,.T.);
#3211=ORIENTED_EDGE('',*,*,#2432,.T.);
#3212=ORIENTED_EDGE('',*,*,#2428,.F.);
#3213=ORIENTED_EDGE('',*,*,#2433,.T.);
#3214=ORIENTED_EDGE('',*,*,#2434,.T.);
#3215=ORIENTED_EDGE('',*,*,#2435,.T.);
#3216=ORIENTED_EDGE('',*,*,#2431,.F.);
#3217=ORIENTED_EDGE('',*,*,#2436,.T.);
#3218=ORIENTED_EDGE('',*,*,#2437,.T.);
#3219=ORIENTED_EDGE('',*,*,#2438,.T.);
#3220=ORIENTED_EDGE('',*,*,#2434,.F.);
#3221=ORIENTED_EDGE('',*,*,#2439,.T.);
#3222=ORIENTED_EDGE('',*,*,#2440,.F.);
#3223=ORIENTED_EDGE('',*,*,#2441,.T.);
#3224=ORIENTED_EDGE('',*,*,#2442,.F.);
#3225=ORIENTED_EDGE('',*,*,#2443,.T.);
#3226=ORIENTED_EDGE('',*,*,#2444,.T.);
#3227=ORIENTED_EDGE('',*,*,#2445,.T.);
#3228=ORIENTED_EDGE('',*,*,#2446,.F.);
#3229=ORIENTED_EDGE('',*,*,#2447,.F.);
#3230=ORIENTED_EDGE('',*,*,#2448,.T.);
#3231=ORIENTED_EDGE('',*,*,#2449,.T.);
#3232=ORIENTED_EDGE('',*,*,#2444,.F.);
#3233=ORIENTED_EDGE('',*,*,#2450,.F.);
#3234=ORIENTED_EDGE('',*,*,#2451,.T.);
#3235=ORIENTED_EDGE('',*,*,#2452,.T.);
#3236=ORIENTED_EDGE('',*,*,#2448,.F.);
#3237=ORIENTED_EDGE('',*,*,#2453,.F.);
#3238=ORIENTED_EDGE('',*,*,#2454,.T.);
#3239=ORIENTED_EDGE('',*,*,#2455,.T.);
#3240=ORIENTED_EDGE('',*,*,#2451,.F.);
#3241=ORIENTED_EDGE('',*,*,#2456,.F.);
#3242=ORIENTED_EDGE('',*,*,#2457,.T.);
#3243=ORIENTED_EDGE('',*,*,#2458,.T.);
#3244=ORIENTED_EDGE('',*,*,#2454,.F.);
#3245=ORIENTED_EDGE('',*,*,#2459,.F.);
#3246=ORIENTED_EDGE('',*,*,#2460,.T.);
#3247=ORIENTED_EDGE('',*,*,#2461,.T.);
#3248=ORIENTED_EDGE('',*,*,#2457,.F.);
#3249=ORIENTED_EDGE('',*,*,#2462,.F.);
#3250=ORIENTED_EDGE('',*,*,#2463,.T.);
#3251=ORIENTED_EDGE('',*,*,#2464,.T.);
#3252=ORIENTED_EDGE('',*,*,#2460,.F.);
#3253=ORIENTED_EDGE('',*,*,#2465,.F.);
#3254=ORIENTED_EDGE('',*,*,#2466,.T.);
#3255=ORIENTED_EDGE('',*,*,#2467,.T.);
#3256=ORIENTED_EDGE('',*,*,#2463,.F.);
#3257=ORIENTED_EDGE('',*,*,#2468,.F.);
#3258=ORIENTED_EDGE('',*,*,#2469,.T.);
#3259=ORIENTED_EDGE('',*,*,#2470,.T.);
#3260=ORIENTED_EDGE('',*,*,#2466,.F.);
#3261=ORIENTED_EDGE('',*,*,#2471,.F.);
#3262=ORIENTED_EDGE('',*,*,#2472,.F.);
#3263=ORIENTED_EDGE('',*,*,#2473,.F.);
#3264=ORIENTED_EDGE('',*,*,#2474,.F.);
#3265=ORIENTED_EDGE('',*,*,#2475,.T.);
#3266=ORIENTED_EDGE('',*,*,#2476,.T.);
#3267=ORIENTED_EDGE('',*,*,#2477,.T.);
#3268=ORIENTED_EDGE('',*,*,#2478,.F.);
#3269=ORIENTED_EDGE('',*,*,#2479,.F.);
#3270=ORIENTED_EDGE('',*,*,#2480,.T.);
#3271=ORIENTED_EDGE('',*,*,#2481,.T.);
#3272=ORIENTED_EDGE('',*,*,#2476,.F.);
#3273=ORIENTED_EDGE('',*,*,#2482,.F.);
#3274=ORIENTED_EDGE('',*,*,#2483,.T.);
#3275=ORIENTED_EDGE('',*,*,#2484,.T.);
#3276=ORIENTED_EDGE('',*,*,#2480,.F.);
#3277=ORIENTED_EDGE('',*,*,#2485,.F.);
#3278=ORIENTED_EDGE('',*,*,#2486,.T.);
#3279=ORIENTED_EDGE('',*,*,#2487,.T.);
#3280=ORIENTED_EDGE('',*,*,#2483,.F.);
#3281=ORIENTED_EDGE('',*,*,#2488,.F.);
#3282=ORIENTED_EDGE('',*,*,#2489,.T.);
#3283=ORIENTED_EDGE('',*,*,#2490,.T.);
#3284=ORIENTED_EDGE('',*,*,#2486,.F.);
#3285=ORIENTED_EDGE('',*,*,#2491,.F.);
#3286=ORIENTED_EDGE('',*,*,#2492,.T.);
#3287=ORIENTED_EDGE('',*,*,#2493,.T.);
#3288=ORIENTED_EDGE('',*,*,#2489,.F.);
#3289=ORIENTED_EDGE('',*,*,#2494,.F.);
#3290=ORIENTED_EDGE('',*,*,#2495,.T.);
#3291=ORIENTED_EDGE('',*,*,#2496,.T.);
#3292=ORIENTED_EDGE('',*,*,#2492,.F.);
#3293=ORIENTED_EDGE('',*,*,#2497,.F.);
#3294=ORIENTED_EDGE('',*,*,#2498,.T.);
#3295=ORIENTED_EDGE('',*,*,#2499,.T.);
#3296=ORIENTED_EDGE('',*,*,#2495,.F.);
#3297=ORIENTED_EDGE('',*,*,#2500,.F.);
#3298=ORIENTED_EDGE('',*,*,#2501,.T.);
#3299=ORIENTED_EDGE('',*,*,#2502,.T.);
#3300=ORIENTED_EDGE('',*,*,#2498,.F.);
#3301=ORIENTED_EDGE('',*,*,#2503,.F.);
#3302=ORIENTED_EDGE('',*,*,#2504,.F.);
#3303=ORIENTED_EDGE('',*,*,#2505,.F.);
#3304=ORIENTED_EDGE('',*,*,#2506,.F.);
#3305=ORIENTED_EDGE('',*,*,#2507,.T.);
#3306=ORIENTED_EDGE('',*,*,#2508,.T.);
#3307=ORIENTED_EDGE('',*,*,#2509,.T.);
#3308=ORIENTED_EDGE('',*,*,#2510,.F.);
#3309=ORIENTED_EDGE('',*,*,#2511,.F.);
#3310=ORIENTED_EDGE('',*,*,#2512,.T.);
#3311=ORIENTED_EDGE('',*,*,#2513,.T.);
#3312=ORIENTED_EDGE('',*,*,#2508,.F.);
#3313=ORIENTED_EDGE('',*,*,#2514,.F.);
#3314=ORIENTED_EDGE('',*,*,#2515,.T.);
#3315=ORIENTED_EDGE('',*,*,#2516,.T.);
#3316=ORIENTED_EDGE('',*,*,#2512,.F.);
#3317=ORIENTED_EDGE('',*,*,#2517,.F.);
#3318=ORIENTED_EDGE('',*,*,#2518,.T.);
#3319=ORIENTED_EDGE('',*,*,#2519,.T.);
#3320=ORIENTED_EDGE('',*,*,#2515,.F.);
#3321=ORIENTED_EDGE('',*,*,#2520,.F.);
#3322=ORIENTED_EDGE('',*,*,#2521,.T.);
#3323=ORIENTED_EDGE('',*,*,#2522,.T.);
#3324=ORIENTED_EDGE('',*,*,#2518,.F.);
#3325=ORIENTED_EDGE('',*,*,#2523,.F.);
#3326=ORIENTED_EDGE('',*,*,#2524,.T.);
#3327=ORIENTED_EDGE('',*,*,#2525,.T.);
#3328=ORIENTED_EDGE('',*,*,#2521,.F.);
#3329=ORIENTED_EDGE('',*,*,#2526,.F.);
#3330=ORIENTED_EDGE('',*,*,#2527,.T.);
#3331=ORIENTED_EDGE('',*,*,#2528,.T.);
#3332=ORIENTED_EDGE('',*,*,#2524,.F.);
#3333=ORIENTED_EDGE('',*,*,#2529,.F.);
#3334=ORIENTED_EDGE('',*,*,#2530,.T.);
#3335=ORIENTED_EDGE('',*,*,#2531,.T.);
#3336=ORIENTED_EDGE('',*,*,#2527,.F.);
#3337=ORIENTED_EDGE('',*,*,#2532,.F.);
#3338=ORIENTED_EDGE('',*,*,#2533,.T.);
#3339=ORIENTED_EDGE('',*,*,#2534,.T.);
#3340=ORIENTED_EDGE('',*,*,#2530,.F.);
#3341=ORIENTED_EDGE('',*,*,#2535,.F.);
#3342=ORIENTED_EDGE('',*,*,#2536,.F.);
#3343=ORIENTED_EDGE('',*,*,#2537,.F.);
#3344=ORIENTED_EDGE('',*,*,#2538,.F.);
#3345=ORIENTED_EDGE('',*,*,#2539,.T.);
#3346=ORIENTED_EDGE('',*,*,#2540,.T.);
#3347=ORIENTED_EDGE('',*,*,#2541,.T.);
#3348=ORIENTED_EDGE('',*,*,#2542,.F.);
#3349=ORIENTED_EDGE('',*,*,#2543,.F.);
#3350=ORIENTED_EDGE('',*,*,#2544,.T.);
#3351=ORIENTED_EDGE('',*,*,#2545,.T.);
#3352=ORIENTED_EDGE('',*,*,#2540,.F.);
#3353=ORIENTED_EDGE('',*,*,#2546,.F.);
#3354=ORIENTED_EDGE('',*,*,#2547,.T.);
#3355=ORIENTED_EDGE('',*,*,#2548,.T.);
#3356=ORIENTED_EDGE('',*,*,#2544,.F.);
#3357=ORIENTED_EDGE('',*,*,#2549,.F.);
#3358=ORIENTED_EDGE('',*,*,#2550,.T.);
#3359=ORIENTED_EDGE('',*,*,#2551,.T.);
#3360=ORIENTED_EDGE('',*,*,#2547,.F.);
#3361=ORIENTED_EDGE('',*,*,#2552,.F.);
#3362=ORIENTED_EDGE('',*,*,#2553,.T.);
#3363=ORIENTED_EDGE('',*,*,#2554,.T.);
#3364=ORIENTED_EDGE('',*,*,#2550,.F.);
#3365=ORIENTED_EDGE('',*,*,#2555,.F.);
#3366=ORIENTED_EDGE('',*,*,#2556,.T.);
#3367=ORIENTED_EDGE('',*,*,#2557,.T.);
#3368=ORIENTED_EDGE('',*,*,#2553,.F.);
#3369=ORIENTED_EDGE('',*,*,#2558,.F.);
#3370=ORIENTED_EDGE('',*,*,#2559,.T.);
#3371=ORIENTED_EDGE('',*,*,#2560,.T.);
#3372=ORIENTED_EDGE('',*,*,#2556,.F.);
#3373=ORIENTED_EDGE('',*,*,#2561,.F.);
#3374=ORIENTED_EDGE('',*,*,#2562,.T.);
#3375=ORIENTED_EDGE('',*,*,#2563,.T.);
#3376=ORIENTED_EDGE('',*,*,#2559,.F.);
#3377=ORIENTED_EDGE('',*,*,#2564,.F.);
#3378=ORIENTED_EDGE('',*,*,#2565,.T.);
#3379=ORIENTED_EDGE('',*,*,#2566,.T.);
#3380=ORIENTED_EDGE('',*,*,#2562,.F.);
#3381=ORIENTED_EDGE('',*,*,#2567,.F.);
#3382=ORIENTED_EDGE('',*,*,#2568,.F.);
#3383=ORIENTED_EDGE('',*,*,#2569,.F.);
#3384=ORIENTED_EDGE('',*,*,#2570,.F.);
#3385=ORIENTED_EDGE('',*,*,#2571,.T.);
#3386=ORIENTED_EDGE('',*,*,#2568,.T.);
#3387=ORIENTED_EDGE('',*,*,#2572,.T.);
#3388=ORIENTED_EDGE('',*,*,#2565,.F.);
#3389=ORIENTED_EDGE('',*,*,#2573,.F.);
#3390=ORIENTED_EDGE('',*,*,#2574,.F.);
#3391=ORIENTED_EDGE('',*,*,#2541,.F.);
#3392=ORIENTED_EDGE('',*,*,#2545,.F.);
#3393=ORIENTED_EDGE('',*,*,#2548,.F.);
#3394=ORIENTED_EDGE('',*,*,#2551,.F.);
#3395=ORIENTED_EDGE('',*,*,#2554,.F.);
#3396=ORIENTED_EDGE('',*,*,#2557,.F.);
#3397=ORIENTED_EDGE('',*,*,#2560,.F.);
#3398=ORIENTED_EDGE('',*,*,#2563,.F.);
#3399=ORIENTED_EDGE('',*,*,#2566,.F.);
#3400=ORIENTED_EDGE('',*,*,#2572,.F.);
#3401=ORIENTED_EDGE('',*,*,#2571,.F.);
#3402=ORIENTED_EDGE('',*,*,#2575,.F.);
#3403=ORIENTED_EDGE('',*,*,#2409,.F.);
#3404=ORIENTED_EDGE('',*,*,#2576,.F.);
#3405=ORIENTED_EDGE('',*,*,#2407,.F.);
#3406=ORIENTED_EDGE('',*,*,#2404,.F.);
#3407=ORIENTED_EDGE('',*,*,#2401,.F.);
#3408=ORIENTED_EDGE('',*,*,#2398,.F.);
#3409=ORIENTED_EDGE('',*,*,#2395,.F.);
#3410=ORIENTED_EDGE('',*,*,#2392,.F.);
#3411=ORIENTED_EDGE('',*,*,#2389,.F.);
#3412=ORIENTED_EDGE('',*,*,#2386,.F.);
#3413=ORIENTED_EDGE('',*,*,#2383,.F.);
#3414=ORIENTED_EDGE('',*,*,#2577,.F.);
#3415=ORIENTED_EDGE('',*,*,#2381,.F.);
#3416=ORIENTED_EDGE('',*,*,#2385,.F.);
#3417=ORIENTED_EDGE('',*,*,#2388,.F.);
#3418=ORIENTED_EDGE('',*,*,#2391,.F.);
#3419=ORIENTED_EDGE('',*,*,#2394,.F.);
#3420=ORIENTED_EDGE('',*,*,#2397,.F.);
#3421=ORIENTED_EDGE('',*,*,#2400,.F.);
#3422=ORIENTED_EDGE('',*,*,#2403,.F.);
#3423=ORIENTED_EDGE('',*,*,#2406,.F.);
#3424=ORIENTED_EDGE('',*,*,#2578,.F.);
#3425=ORIENTED_EDGE('',*,*,#2411,.F.);
#3426=ORIENTED_EDGE('',*,*,#2579,.F.);
#3427=ORIENTED_EDGE('',*,*,#2569,.T.);
#3428=ORIENTED_EDGE('',*,*,#2573,.T.);
#3429=ORIENTED_EDGE('',*,*,#2567,.T.);
#3430=ORIENTED_EDGE('',*,*,#2564,.T.);
#3431=ORIENTED_EDGE('',*,*,#2561,.T.);
#3432=ORIENTED_EDGE('',*,*,#2558,.T.);
#3433=ORIENTED_EDGE('',*,*,#2555,.T.);
#3434=ORIENTED_EDGE('',*,*,#2552,.T.);
#3435=ORIENTED_EDGE('',*,*,#2549,.T.);
#3436=ORIENTED_EDGE('',*,*,#2546,.T.);
#3437=ORIENTED_EDGE('',*,*,#2543,.T.);
#3438=ORIENTED_EDGE('',*,*,#2580,.T.);
#3439=ORIENTED_EDGE('',*,*,#2581,.T.);
#3440=ORIENTED_EDGE('',*,*,#2582,.T.);
#3441=ORIENTED_EDGE('',*,*,#2583,.T.);
#3442=ORIENTED_EDGE('',*,*,#2584,.T.);
#3443=ORIENTED_EDGE('',*,*,#2538,.T.);
#3444=ORIENTED_EDGE('',*,*,#2585,.T.);
#3445=ORIENTED_EDGE('',*,*,#2442,.T.);
#3446=ORIENTED_EDGE('',*,*,#2575,.T.);
#3447=ORIENTED_EDGE('',*,*,#2570,.T.);
#3448=ORIENTED_EDGE('',*,*,#2579,.T.);
#3449=ORIENTED_EDGE('',*,*,#2410,.T.);
#3450=ORIENTED_EDGE('',*,*,#2586,.T.);
#3451=ORIENTED_EDGE('',*,*,#2506,.T.);
#3452=ORIENTED_EDGE('',*,*,#2587,.T.);
#3453=ORIENTED_EDGE('',*,*,#2378,.T.);
#3454=ORIENTED_EDGE('',*,*,#2588,.T.);
#3455=ORIENTED_EDGE('',*,*,#2474,.T.);
#3456=ORIENTED_EDGE('',*,*,#2589,.T.);
#3457=ORIENTED_EDGE('',*,*,#2346,.T.);
#3458=ORIENTED_EDGE('',*,*,#2536,.T.);
#3459=ORIENTED_EDGE('',*,*,#2590,.T.);
#3460=ORIENTED_EDGE('',*,*,#2533,.F.);
#3461=ORIENTED_EDGE('',*,*,#2591,.F.);
#3462=ORIENTED_EDGE('',*,*,#2592,.F.);
#3463=ORIENTED_EDGE('',*,*,#2509,.F.);
#3464=ORIENTED_EDGE('',*,*,#2513,.F.);
#3465=ORIENTED_EDGE('',*,*,#2516,.F.);
#3466=ORIENTED_EDGE('',*,*,#2519,.F.);
#3467=ORIENTED_EDGE('',*,*,#2522,.F.);
#3468=ORIENTED_EDGE('',*,*,#2525,.F.);
#3469=ORIENTED_EDGE('',*,*,#2528,.F.);
#3470=ORIENTED_EDGE('',*,*,#2531,.F.);
#3471=ORIENTED_EDGE('',*,*,#2534,.F.);
#3472=ORIENTED_EDGE('',*,*,#2590,.F.);
#3473=ORIENTED_EDGE('',*,*,#2539,.F.);
#3474=ORIENTED_EDGE('',*,*,#2584,.F.);
#3475=ORIENTED_EDGE('',*,*,#2441,.F.);
#3476=ORIENTED_EDGE('',*,*,#2593,.F.);
#3477=ORIENTED_EDGE('',*,*,#2439,.F.);
#3478=ORIENTED_EDGE('',*,*,#2436,.F.);
#3479=ORIENTED_EDGE('',*,*,#2433,.F.);
#3480=ORIENTED_EDGE('',*,*,#2430,.F.);
#3481=ORIENTED_EDGE('',*,*,#2427,.F.);
#3482=ORIENTED_EDGE('',*,*,#2424,.F.);
#3483=ORIENTED_EDGE('',*,*,#2421,.F.);
#3484=ORIENTED_EDGE('',*,*,#2418,.F.);
#3485=ORIENTED_EDGE('',*,*,#2415,.F.);
#3486=ORIENTED_EDGE('',*,*,#2594,.F.);
#3487=ORIENTED_EDGE('',*,*,#2413,.F.);
#3488=ORIENTED_EDGE('',*,*,#2417,.F.);
#3489=ORIENTED_EDGE('',*,*,#2420,.F.);
#3490=ORIENTED_EDGE('',*,*,#2423,.F.);
#3491=ORIENTED_EDGE('',*,*,#2426,.F.);
#3492=ORIENTED_EDGE('',*,*,#2429,.F.);
#3493=ORIENTED_EDGE('',*,*,#2432,.F.);
#3494=ORIENTED_EDGE('',*,*,#2435,.F.);
#3495=ORIENTED_EDGE('',*,*,#2438,.F.);
#3496=ORIENTED_EDGE('',*,*,#2595,.F.);
#3497=ORIENTED_EDGE('',*,*,#2443,.F.);
#3498=ORIENTED_EDGE('',*,*,#2585,.F.);
#3499=ORIENTED_EDGE('',*,*,#2537,.T.);
#3500=ORIENTED_EDGE('',*,*,#2591,.T.);
#3501=ORIENTED_EDGE('',*,*,#2535,.T.);
#3502=ORIENTED_EDGE('',*,*,#2532,.T.);
#3503=ORIENTED_EDGE('',*,*,#2529,.T.);
#3504=ORIENTED_EDGE('',*,*,#2526,.T.);
#3505=ORIENTED_EDGE('',*,*,#2523,.T.);
#3506=ORIENTED_EDGE('',*,*,#2520,.T.);
#3507=ORIENTED_EDGE('',*,*,#2517,.T.);
#3508=ORIENTED_EDGE('',*,*,#2514,.T.);
#3509=ORIENTED_EDGE('',*,*,#2511,.T.);
#3510=ORIENTED_EDGE('',*,*,#2504,.T.);
#3511=ORIENTED_EDGE('',*,*,#2596,.T.);
#3512=ORIENTED_EDGE('',*,*,#2501,.F.);
#3513=ORIENTED_EDGE('',*,*,#2597,.F.);
#3514=ORIENTED_EDGE('',*,*,#2598,.F.);
#3515=ORIENTED_EDGE('',*,*,#2477,.F.);
#3516=ORIENTED_EDGE('',*,*,#2481,.F.);
#3517=ORIENTED_EDGE('',*,*,#2484,.F.);
#3518=ORIENTED_EDGE('',*,*,#2487,.F.);
#3519=ORIENTED_EDGE('',*,*,#2490,.F.);
#3520=ORIENTED_EDGE('',*,*,#2493,.F.);
#3521=ORIENTED_EDGE('',*,*,#2496,.F.);
#3522=ORIENTED_EDGE('',*,*,#2499,.F.);
#3523=ORIENTED_EDGE('',*,*,#2502,.F.);
#3524=ORIENTED_EDGE('',*,*,#2596,.F.);
#3525=ORIENTED_EDGE('',*,*,#2507,.F.);
#3526=ORIENTED_EDGE('',*,*,#2586,.F.);
#3527=ORIENTED_EDGE('',*,*,#2377,.F.);
#3528=ORIENTED_EDGE('',*,*,#2599,.F.);
#3529=ORIENTED_EDGE('',*,*,#2375,.F.);
#3530=ORIENTED_EDGE('',*,*,#2372,.F.);
#3531=ORIENTED_EDGE('',*,*,#2369,.F.);
#3532=ORIENTED_EDGE('',*,*,#2366,.F.);
#3533=ORIENTED_EDGE('',*,*,#2363,.F.);
#3534=ORIENTED_EDGE('',*,*,#2360,.F.);
#3535=ORIENTED_EDGE('',*,*,#2357,.F.);
#3536=ORIENTED_EDGE('',*,*,#2354,.F.);
#3537=ORIENTED_EDGE('',*,*,#2351,.F.);
#3538=ORIENTED_EDGE('',*,*,#2600,.F.);
#3539=ORIENTED_EDGE('',*,*,#2349,.F.);
#3540=ORIENTED_EDGE('',*,*,#2353,.F.);
#3541=ORIENTED_EDGE('',*,*,#2356,.F.);
#3542=ORIENTED_EDGE('',*,*,#2359,.F.);
#3543=ORIENTED_EDGE('',*,*,#2362,.F.);
#3544=ORIENTED_EDGE('',*,*,#2365,.F.);
#3545=ORIENTED_EDGE('',*,*,#2368,.F.);
#3546=ORIENTED_EDGE('',*,*,#2371,.F.);
#3547=ORIENTED_EDGE('',*,*,#2374,.F.);
#3548=ORIENTED_EDGE('',*,*,#2601,.F.);
#3549=ORIENTED_EDGE('',*,*,#2379,.F.);
#3550=ORIENTED_EDGE('',*,*,#2587,.F.);
#3551=ORIENTED_EDGE('',*,*,#2505,.T.);
#3552=ORIENTED_EDGE('',*,*,#2597,.T.);
#3553=ORIENTED_EDGE('',*,*,#2503,.T.);
#3554=ORIENTED_EDGE('',*,*,#2500,.T.);
#3555=ORIENTED_EDGE('',*,*,#2497,.T.);
#3556=ORIENTED_EDGE('',*,*,#2494,.T.);
#3557=ORIENTED_EDGE('',*,*,#2491,.T.);
#3558=ORIENTED_EDGE('',*,*,#2488,.T.);
#3559=ORIENTED_EDGE('',*,*,#2485,.T.);
#3560=ORIENTED_EDGE('',*,*,#2482,.T.);
#3561=ORIENTED_EDGE('',*,*,#2479,.T.);
#3562=ORIENTED_EDGE('',*,*,#2472,.T.);
#3563=ORIENTED_EDGE('',*,*,#2602,.T.);
#3564=ORIENTED_EDGE('',*,*,#2469,.F.);
#3565=ORIENTED_EDGE('',*,*,#2603,.F.);
#3566=ORIENTED_EDGE('',*,*,#2604,.F.);
#3567=ORIENTED_EDGE('',*,*,#2445,.F.);
#3568=ORIENTED_EDGE('',*,*,#2449,.F.);
#3569=ORIENTED_EDGE('',*,*,#2452,.F.);
#3570=ORIENTED_EDGE('',*,*,#2455,.F.);
#3571=ORIENTED_EDGE('',*,*,#2458,.F.);
#3572=ORIENTED_EDGE('',*,*,#2461,.F.);
#3573=ORIENTED_EDGE('',*,*,#2464,.F.);
#3574=ORIENTED_EDGE('',*,*,#2467,.F.);
#3575=ORIENTED_EDGE('',*,*,#2470,.F.);
#3576=ORIENTED_EDGE('',*,*,#2602,.F.);
#3577=ORIENTED_EDGE('',*,*,#2475,.F.);
#3578=ORIENTED_EDGE('',*,*,#2588,.F.);
#3579=ORIENTED_EDGE('',*,*,#2345,.F.);
#3580=ORIENTED_EDGE('',*,*,#2605,.F.);
#3581=ORIENTED_EDGE('',*,*,#2343,.F.);
#3582=ORIENTED_EDGE('',*,*,#2340,.F.);
#3583=ORIENTED_EDGE('',*,*,#2337,.F.);
#3584=ORIENTED_EDGE('',*,*,#2334,.F.);
#3585=ORIENTED_EDGE('',*,*,#2331,.F.);
#3586=ORIENTED_EDGE('',*,*,#2328,.F.);
#3587=ORIENTED_EDGE('',*,*,#2325,.F.);
#3588=ORIENTED_EDGE('',*,*,#2322,.F.);
#3589=ORIENTED_EDGE('',*,*,#2319,.F.);
#3590=ORIENTED_EDGE('',*,*,#2606,.F.);
#3591=ORIENTED_EDGE('',*,*,#2317,.F.);
#3592=ORIENTED_EDGE('',*,*,#2321,.F.);
#3593=ORIENTED_EDGE('',*,*,#2324,.F.);
#3594=ORIENTED_EDGE('',*,*,#2327,.F.);
#3595=ORIENTED_EDGE('',*,*,#2330,.F.);
#3596=ORIENTED_EDGE('',*,*,#2333,.F.);
#3597=ORIENTED_EDGE('',*,*,#2336,.F.);
#3598=ORIENTED_EDGE('',*,*,#2339,.F.);
#3599=ORIENTED_EDGE('',*,*,#2342,.F.);
#3600=ORIENTED_EDGE('',*,*,#2607,.F.);
#3601=ORIENTED_EDGE('',*,*,#2347,.F.);
#3602=ORIENTED_EDGE('',*,*,#2589,.F.);
#3603=ORIENTED_EDGE('',*,*,#2473,.T.);
#3604=ORIENTED_EDGE('',*,*,#2603,.T.);
#3605=ORIENTED_EDGE('',*,*,#2471,.T.);
#3606=ORIENTED_EDGE('',*,*,#2468,.T.);
#3607=ORIENTED_EDGE('',*,*,#2465,.T.);
#3608=ORIENTED_EDGE('',*,*,#2462,.T.);
#3609=ORIENTED_EDGE('',*,*,#2459,.T.);
#3610=ORIENTED_EDGE('',*,*,#2456,.T.);
#3611=ORIENTED_EDGE('',*,*,#2453,.T.);
#3612=ORIENTED_EDGE('',*,*,#2450,.T.);
#3613=ORIENTED_EDGE('',*,*,#2447,.T.);
#3614=ORIENTED_EDGE('',*,*,#2440,.T.);
#3615=ORIENTED_EDGE('',*,*,#2595,.T.);
#3616=ORIENTED_EDGE('',*,*,#2437,.F.);
#3617=ORIENTED_EDGE('',*,*,#2593,.T.);
#3618=ORIENTED_EDGE('',*,*,#2408,.T.);
#3619=ORIENTED_EDGE('',*,*,#2578,.T.);
#3620=ORIENTED_EDGE('',*,*,#2405,.F.);
#3621=ORIENTED_EDGE('',*,*,#2576,.T.);
#3622=ORIENTED_EDGE('',*,*,#2376,.T.);
#3623=ORIENTED_EDGE('',*,*,#2601,.T.);
#3624=ORIENTED_EDGE('',*,*,#2373,.F.);
#3625=ORIENTED_EDGE('',*,*,#2599,.T.);
#3626=ORIENTED_EDGE('',*,*,#2344,.T.);
#3627=ORIENTED_EDGE('',*,*,#2607,.T.);
#3628=ORIENTED_EDGE('',*,*,#2341,.F.);
#3629=ORIENTED_EDGE('',*,*,#2605,.T.);
#3630=ORIENTED_EDGE('',*,*,#2608,.T.);
#3631=ORIENTED_EDGE('',*,*,#2609,.T.);
#3632=ORIENTED_EDGE('',*,*,#2583,.F.);
#3633=ORIENTED_EDGE('',*,*,#2610,.F.);
#3634=ORIENTED_EDGE('',*,*,#2611,.T.);
#3635=ORIENTED_EDGE('',*,*,#2610,.T.);
#3636=ORIENTED_EDGE('',*,*,#2582,.F.);
#3637=ORIENTED_EDGE('',*,*,#2612,.F.);
#3638=ORIENTED_EDGE('',*,*,#2613,.T.);
#3639=ORIENTED_EDGE('',*,*,#2612,.T.);
#3640=ORIENTED_EDGE('',*,*,#2581,.F.);
#3641=ORIENTED_EDGE('',*,*,#2614,.F.);
#3642=ORIENTED_EDGE('',*,*,#2615,.T.);
#3643=ORIENTED_EDGE('',*,*,#2614,.T.);
#3644=ORIENTED_EDGE('',*,*,#2580,.F.);
#3645=ORIENTED_EDGE('',*,*,#2609,.F.);
#3646=ORIENTED_EDGE('',*,*,#2615,.F.);
#3647=ORIENTED_EDGE('',*,*,#2608,.F.);
#3648=ORIENTED_EDGE('',*,*,#2611,.F.);
#3649=ORIENTED_EDGE('',*,*,#2613,.F.);
#3650=ORIENTED_EDGE('',*,*,#2574,.T.);
#3651=ORIENTED_EDGE('',*,*,#2382,.T.);
#3652=ORIENTED_EDGE('',*,*,#2577,.T.);
#3653=ORIENTED_EDGE('',*,*,#2542,.T.);
#3654=ORIENTED_EDGE('',*,*,#2592,.T.);
#3655=ORIENTED_EDGE('',*,*,#2414,.T.);
#3656=ORIENTED_EDGE('',*,*,#2594,.T.);
#3657=ORIENTED_EDGE('',*,*,#2510,.T.);
#3658=ORIENTED_EDGE('',*,*,#2598,.T.);
#3659=ORIENTED_EDGE('',*,*,#2350,.T.);
#3660=ORIENTED_EDGE('',*,*,#2600,.T.);
#3661=ORIENTED_EDGE('',*,*,#2478,.T.);
#3662=ORIENTED_EDGE('',*,*,#2604,.T.);
#3663=ORIENTED_EDGE('',*,*,#2318,.T.);
#3664=ORIENTED_EDGE('',*,*,#2606,.T.);
#3665=ORIENTED_EDGE('',*,*,#2446,.T.);
#3666=ORIENTED_EDGE('',*,*,#2616,.T.);
#3667=ORIENTED_EDGE('',*,*,#2617,.T.);
#3668=ORIENTED_EDGE('',*,*,#2618,.F.);
#3669=ORIENTED_EDGE('',*,*,#2619,.F.);
#3670=ORIENTED_EDGE('',*,*,#2620,.T.);
#3671=ORIENTED_EDGE('',*,*,#2619,.T.);
#3672=ORIENTED_EDGE('',*,*,#2621,.F.);
#3673=ORIENTED_EDGE('',*,*,#2622,.F.);
#3674=ORIENTED_EDGE('',*,*,#2623,.T.);
#3675=ORIENTED_EDGE('',*,*,#2622,.T.);
#3676=ORIENTED_EDGE('',*,*,#2624,.F.);
#3677=ORIENTED_EDGE('',*,*,#2625,.F.);
#3678=ORIENTED_EDGE('',*,*,#2626,.T.);
#3679=ORIENTED_EDGE('',*,*,#2625,.T.);
#3680=ORIENTED_EDGE('',*,*,#2627,.F.);
#3681=ORIENTED_EDGE('',*,*,#2617,.F.);
#3682=ORIENTED_EDGE('',*,*,#2627,.T.);
#3683=ORIENTED_EDGE('',*,*,#2624,.T.);
#3684=ORIENTED_EDGE('',*,*,#2621,.T.);
#3685=ORIENTED_EDGE('',*,*,#2618,.T.);
#3686=ORIENTED_EDGE('',*,*,#2626,.F.);
#3687=ORIENTED_EDGE('',*,*,#2616,.F.);
#3688=ORIENTED_EDGE('',*,*,#2620,.F.);
#3689=ORIENTED_EDGE('',*,*,#2623,.F.);
#3690=ORIENTED_EDGE('',*,*,#2628,.F.);
#3691=ORIENTED_EDGE('',*,*,#2629,.T.);
#3692=ORIENTED_EDGE('',*,*,#2630,.T.);
#3693=ORIENTED_EDGE('',*,*,#2629,.F.);
#3694=ORIENTED_EDGE('',*,*,#2631,.F.);
#3695=ORIENTED_EDGE('',*,*,#2632,.T.);
#3696=ORIENTED_EDGE('',*,*,#2633,.T.);
#3697=ORIENTED_EDGE('',*,*,#2632,.F.);
#3698=ORIENTED_EDGE('',*,*,#2631,.T.);
#3699=ORIENTED_EDGE('',*,*,#2628,.T.);
#3700=ORIENTED_EDGE('',*,*,#2633,.F.);
#3701=ORIENTED_EDGE('',*,*,#2630,.F.);
#3702=ORIENTED_EDGE('',*,*,#2634,.F.);
#3703=ORIENTED_EDGE('',*,*,#2635,.T.);
#3704=ORIENTED_EDGE('',*,*,#2636,.T.);
#3705=ORIENTED_EDGE('',*,*,#2635,.F.);
#3706=ORIENTED_EDGE('',*,*,#2637,.F.);
#3707=ORIENTED_EDGE('',*,*,#2638,.T.);
#3708=ORIENTED_EDGE('',*,*,#2639,.T.);
#3709=ORIENTED_EDGE('',*,*,#2638,.F.);
#3710=ORIENTED_EDGE('',*,*,#2637,.T.);
#3711=ORIENTED_EDGE('',*,*,#2634,.T.);
#3712=ORIENTED_EDGE('',*,*,#2639,.F.);
#3713=ORIENTED_EDGE('',*,*,#2636,.F.);
#3714=ORIENTED_EDGE('',*,*,#2640,.T.);
#3715=ORIENTED_EDGE('',*,*,#2641,.T.);
#3716=ORIENTED_EDGE('',*,*,#2642,.F.);
#3717=ORIENTED_EDGE('',*,*,#2641,.F.);
#3718=ORIENTED_EDGE('',*,*,#2643,.F.);
#3719=ORIENTED_EDGE('',*,*,#2640,.F.);
#3720=ORIENTED_EDGE('',*,*,#2644,.F.);
#3721=ORIENTED_EDGE('',*,*,#2642,.T.);
#3722=ORIENTED_EDGE('',*,*,#2645,.F.);
#3723=ORIENTED_EDGE('',*,*,#2646,.T.);
#3724=ORIENTED_EDGE('',*,*,#2644,.T.);
#3725=ORIENTED_EDGE('',*,*,#2646,.F.);
#3726=ORIENTED_EDGE('',*,*,#2647,.T.);
#3727=ORIENTED_EDGE('',*,*,#2648,.F.);
#3728=ORIENTED_EDGE('',*,*,#2647,.F.);
#3729=ORIENTED_EDGE('',*,*,#2649,.T.);
#3730=ORIENTED_EDGE('',*,*,#2650,.T.);
#3731=ORIENTED_EDGE('',*,*,#2649,.F.);
#3732=ORIENTED_EDGE('',*,*,#2650,.F.);
#3733=ORIENTED_EDGE('',*,*,#2643,.T.);
#3734=ORIENTED_EDGE('',*,*,#2651,.T.);
#3735=ORIENTED_EDGE('',*,*,#2648,.T.);
#3736=ORIENTED_EDGE('',*,*,#2651,.F.);
#3737=ORIENTED_EDGE('',*,*,#2645,.T.);
#3738=ORIENTED_EDGE('',*,*,#2652,.F.);
#3739=ORIENTED_EDGE('',*,*,#2653,.F.);
#3740=ORIENTED_EDGE('',*,*,#2654,.F.);
#3741=ORIENTED_EDGE('',*,*,#2655,.F.);
#3742=ORIENTED_EDGE('',*,*,#2656,.F.);
#3743=ORIENTED_EDGE('',*,*,#2657,.F.);
#3744=ORIENTED_EDGE('',*,*,#2658,.F.);
#3745=ORIENTED_EDGE('',*,*,#2659,.F.);
#3746=ORIENTED_EDGE('',*,*,#2659,.T.);
#3747=ORIENTED_EDGE('',*,*,#2660,.F.);
#3748=ORIENTED_EDGE('',*,*,#2653,.T.);
#3749=ORIENTED_EDGE('',*,*,#2661,.F.);
#3750=ORIENTED_EDGE('',*,*,#2656,.T.);
#3751=ORIENTED_EDGE('',*,*,#2661,.T.);
#3752=ORIENTED_EDGE('',*,*,#2652,.T.);
#3753=ORIENTED_EDGE('',*,*,#2662,.F.);
#3754=ORIENTED_EDGE('',*,*,#2658,.T.);
#3755=ORIENTED_EDGE('',*,*,#2663,.F.);
#3756=ORIENTED_EDGE('',*,*,#2654,.T.);
#3757=ORIENTED_EDGE('',*,*,#2660,.T.);
#3758=ORIENTED_EDGE('',*,*,#2657,.T.);
#3759=ORIENTED_EDGE('',*,*,#2662,.T.);
#3760=ORIENTED_EDGE('',*,*,#2655,.T.);
#3761=ORIENTED_EDGE('',*,*,#2663,.T.);
#3762=ORIENTED_EDGE('',*,*,#2664,.F.);
#3763=ORIENTED_EDGE('',*,*,#2665,.T.);
#3764=ORIENTED_EDGE('',*,*,#2666,.T.);
#3765=ORIENTED_EDGE('',*,*,#2665,.F.);
#3766=ORIENTED_EDGE('',*,*,#2667,.F.);
#3767=ORIENTED_EDGE('',*,*,#2668,.T.);
#3768=ORIENTED_EDGE('',*,*,#2669,.T.);
#3769=ORIENTED_EDGE('',*,*,#2668,.F.);
#3770=ORIENTED_EDGE('',*,*,#2667,.T.);
#3771=ORIENTED_EDGE('',*,*,#2664,.T.);
#3772=ORIENTED_EDGE('',*,*,#2669,.F.);
#3773=ORIENTED_EDGE('',*,*,#2666,.F.);
#3774=ORIENTED_EDGE('',*,*,#2670,.F.);
#3775=ORIENTED_EDGE('',*,*,#2671,.T.);
#3776=ORIENTED_EDGE('',*,*,#2672,.T.);
#3777=ORIENTED_EDGE('',*,*,#2671,.F.);
#3778=ORIENTED_EDGE('',*,*,#2673,.F.);
#3779=ORIENTED_EDGE('',*,*,#2674,.T.);
#3780=ORIENTED_EDGE('',*,*,#2675,.T.);
#3781=ORIENTED_EDGE('',*,*,#2674,.F.);
#3782=ORIENTED_EDGE('',*,*,#2673,.T.);
#3783=ORIENTED_EDGE('',*,*,#2670,.T.);
#3784=ORIENTED_EDGE('',*,*,#2675,.F.);
#3785=ORIENTED_EDGE('',*,*,#2672,.F.);
#3786=ORIENTED_EDGE('',*,*,#2676,.F.);
#3787=ORIENTED_EDGE('',*,*,#2677,.T.);
#3788=ORIENTED_EDGE('',*,*,#2678,.T.);
#3789=ORIENTED_EDGE('',*,*,#2677,.F.);
#3790=ORIENTED_EDGE('',*,*,#2679,.F.);
#3791=ORIENTED_EDGE('',*,*,#2680,.T.);
#3792=ORIENTED_EDGE('',*,*,#2681,.T.);
#3793=ORIENTED_EDGE('',*,*,#2680,.F.);
#3794=ORIENTED_EDGE('',*,*,#2679,.T.);
#3795=ORIENTED_EDGE('',*,*,#2676,.T.);
#3796=ORIENTED_EDGE('',*,*,#2681,.F.);
#3797=ORIENTED_EDGE('',*,*,#2678,.F.);
#3798=CYLINDRICAL_SURFACE('',#4346,1.);
#3799=CYLINDRICAL_SURFACE('',#4358,1.);
#3800=CYLINDRICAL_SURFACE('',#4361,1.);
#3801=CYLINDRICAL_SURFACE('',#4363,1.);
#3802=CYLINDRICAL_SURFACE('',#4365,1.);
#3803=CYLINDRICAL_SURFACE('',#4368,1.);
#3804=CYLINDRICAL_SURFACE('',#4371,1.);
#3805=CYLINDRICAL_SURFACE('',#4374,1.);
#3806=CYLINDRICAL_SURFACE('',#4381,1.);
#3807=CYLINDRICAL_SURFACE('',#4393,1.);
#3808=CYLINDRICAL_SURFACE('',#4396,1.);
#3809=CYLINDRICAL_SURFACE('',#4398,1.);
#3810=CYLINDRICAL_SURFACE('',#4400,1.);
#3811=CYLINDRICAL_SURFACE('',#4403,1.);
#3812=CYLINDRICAL_SURFACE('',#4406,1.);
#3813=CYLINDRICAL_SURFACE('',#4409,1.);
#3814=CYLINDRICAL_SURFACE('',#4416,7.);
#3815=CYLINDRICAL_SURFACE('',#4419,7.);
#3816=CYLINDRICAL_SURFACE('',#4422,7.);
#3817=CYLINDRICAL_SURFACE('',#4425,7.);
#3818=CYLINDRICAL_SURFACE('',#4435,7.);
#3819=CYLINDRICAL_SURFACE('',#4438,7.);
#3820=CYLINDRICAL_SURFACE('',#4441,7.);
#3821=CYLINDRICAL_SURFACE('',#4444,7.);
#3822=CYLINDRICAL_SURFACE('',#4468,6.);
#3823=CYLINDRICAL_SURFACE('',#4471,6.);
#3824=CYLINDRICAL_SURFACE('',#4474,6.);
#3825=CYLINDRICAL_SURFACE('',#4477,6.);
#3826=CYLINDRICAL_SURFACE('',#4487,2.5175);
#3827=CYLINDRICAL_SURFACE('',#4489,2.5175);
#3828=CYLINDRICAL_SURFACE('',#4490,2.5175);
#3829=CYLINDRICAL_SURFACE('',#4491,2.5175);
#3830=CYLINDRICAL_SURFACE('',#4492,2.5175);
#3831=CYLINDRICAL_SURFACE('',#4493,2.5175);
#3832=CYLINDRICAL_SURFACE('',#4494,2.5175);
#3833=CYLINDRICAL_SURFACE('',#4495,2.5175);
#3834=CYLINDRICAL_SURFACE('',#4496,2.5175);
#3835=CYLINDRICAL_SURFACE('',#4497,2.5175);
#3836=CYLINDRICAL_SURFACE('',#4499,2.5175);
#3837=CYLINDRICAL_SURFACE('',#4501,2.5175);
#3838=CYLINDRICAL_SURFACE('',#4502,2.5175);
#3839=CYLINDRICAL_SURFACE('',#4503,2.5175);
#3840=CYLINDRICAL_SURFACE('',#4504,2.5175);
#3841=CYLINDRICAL_SURFACE('',#4505,2.5175);
#3842=CYLINDRICAL_SURFACE('',#4506,2.5175);
#3843=CYLINDRICAL_SURFACE('',#4507,2.5175);
#3844=CYLINDRICAL_SURFACE('',#4508,2.5175);
#3845=CYLINDRICAL_SURFACE('',#4509,2.5175);
#3846=CYLINDRICAL_SURFACE('',#4511,2.5175);
#3847=CYLINDRICAL_SURFACE('',#4513,2.5175);
#3848=CYLINDRICAL_SURFACE('',#4514,2.5175);
#3849=CYLINDRICAL_SURFACE('',#4515,2.5175);
#3850=CYLINDRICAL_SURFACE('',#4516,2.5175);
#3851=CYLINDRICAL_SURFACE('',#4517,2.5175);
#3852=CYLINDRICAL_SURFACE('',#4518,2.5175);
#3853=CYLINDRICAL_SURFACE('',#4519,2.5175);
#3854=CYLINDRICAL_SURFACE('',#4520,2.5175);
#3855=CYLINDRICAL_SURFACE('',#4521,2.5175);
#3856=CYLINDRICAL_SURFACE('',#4523,2.5175);
#3857=CYLINDRICAL_SURFACE('',#4525,2.5175);
#3858=CYLINDRICAL_SURFACE('',#4526,2.5175);
#3859=CYLINDRICAL_SURFACE('',#4527,2.5175);
#3860=CYLINDRICAL_SURFACE('',#4528,2.5175);
#3861=CYLINDRICAL_SURFACE('',#4529,2.5175);
#3862=CYLINDRICAL_SURFACE('',#4530,2.5175);
#3863=CYLINDRICAL_SURFACE('',#4531,2.5175);
#3864=CYLINDRICAL_SURFACE('',#4532,2.5175);
#3865=CYLINDRICAL_SURFACE('',#4533,2.5175);
#3866=CYLINDRICAL_SURFACE('',#4535,3.0735);
#3867=CYLINDRICAL_SURFACE('',#4537,3.0735);
#3868=CYLINDRICAL_SURFACE('',#4538,3.0735);
#3869=CYLINDRICAL_SURFACE('',#4539,3.0735);
#3870=CYLINDRICAL_SURFACE('',#4540,3.0735);
#3871=CYLINDRICAL_SURFACE('',#4541,3.0735);
#3872=CYLINDRICAL_SURFACE('',#4542,3.0735);
#3873=CYLINDRICAL_SURFACE('',#4543,3.0735);
#3874=CYLINDRICAL_SURFACE('',#4544,3.0735);
#3875=CYLINDRICAL_SURFACE('',#4545,3.0735);
#3876=CYLINDRICAL_SURFACE('',#4547,3.07350000000001);
#3877=CYLINDRICAL_SURFACE('',#4549,3.07350000000001);
#3878=CYLINDRICAL_SURFACE('',#4550,3.07350000000001);
#3879=CYLINDRICAL_SURFACE('',#4551,3.07350000000001);
#3880=CYLINDRICAL_SURFACE('',#4552,3.07350000000001);
#3881=CYLINDRICAL_SURFACE('',#4553,3.07350000000001);
#3882=CYLINDRICAL_SURFACE('',#4554,3.07350000000001);
#3883=CYLINDRICAL_SURFACE('',#4555,3.07350000000001);
#3884=CYLINDRICAL_SURFACE('',#4556,3.07350000000001);
#3885=CYLINDRICAL_SURFACE('',#4557,3.07350000000001);
#3886=CYLINDRICAL_SURFACE('',#4559,3.0735);
#3887=CYLINDRICAL_SURFACE('',#4561,3.0735);
#3888=CYLINDRICAL_SURFACE('',#4562,3.0735);
#3889=CYLINDRICAL_SURFACE('',#4563,3.0735);
#3890=CYLINDRICAL_SURFACE('',#4564,3.0735);
#3891=CYLINDRICAL_SURFACE('',#4565,3.0735);
#3892=CYLINDRICAL_SURFACE('',#4566,3.0735);
#3893=CYLINDRICAL_SURFACE('',#4567,3.0735);
#3894=CYLINDRICAL_SURFACE('',#4568,3.0735);
#3895=CYLINDRICAL_SURFACE('',#4569,3.0735);
#3896=CYLINDRICAL_SURFACE('',#4571,3.07350000000001);
#3897=CYLINDRICAL_SURFACE('',#4573,3.07350000000001);
#3898=CYLINDRICAL_SURFACE('',#4574,3.07350000000001);
#3899=CYLINDRICAL_SURFACE('',#4575,3.07350000000001);
#3900=CYLINDRICAL_SURFACE('',#4576,3.07350000000001);
#3901=CYLINDRICAL_SURFACE('',#4577,3.07350000000001);
#3902=CYLINDRICAL_SURFACE('',#4578,3.07350000000001);
#3903=CYLINDRICAL_SURFACE('',#4579,3.07350000000001);
#3904=CYLINDRICAL_SURFACE('',#4580,3.07350000000001);
#3905=CYLINDRICAL_SURFACE('',#4581,3.07350000000001);
#3906=CYLINDRICAL_SURFACE('',#4583,3.07350000000001);
#3907=CYLINDRICAL_SURFACE('',#4585,3.0735);
#3908=CYLINDRICAL_SURFACE('',#4586,3.07350000000001);
#3909=CYLINDRICAL_SURFACE('',#4587,3.0735);
#3910=CYLINDRICAL_SURFACE('',#4588,2.5175);
#3911=CYLINDRICAL_SURFACE('',#4589,2.5175);
#3912=CYLINDRICAL_SURFACE('',#4590,2.5175);
#3913=CYLINDRICAL_SURFACE('',#4591,2.5175);
#3914=CYLINDRICAL_SURFACE('',#4605,8.);
#3915=CYLINDRICAL_SURFACE('',#4608,15.);
#3916=CYLINDRICAL_SURFACE('',#4614,6.);
#3917=CYLINDRICAL_SURFACE('',#4617,8.);
#3918=CYLINDRICAL_SURFACE('',#4623,5.);
#3919=CYLINDRICAL_SURFACE('',#4630,6.);
#3920=CYLINDRICAL_SURFACE('',#4635,9.);
#3921=CYLINDRICAL_SURFACE('',#4638,6.);
#3922=CYLINDRICAL_SURFACE('',#4646,5.);
#3923=CYLINDRICAL_SURFACE('',#4648,9.);
#3924=CYLINDRICAL_SURFACE('',#4652,6.);
#3925=CYLINDRICAL_SURFACE('',#4655,10.);
#3926=CYLINDRICAL_SURFACE('',#4661,6.);
#3927=CYLINDRICAL_SURFACE('',#4664,11.);
#3928=CYLINDRICAL_SURFACE('',#4670,6.);
#3929=CYLINDRICAL_SURFACE('',#4673,11.);
#3930=ADVANCED_FACE('',(#633),#3798,.T.);
#3931=ADVANCED_FACE('',(#634),#552,.T.);
#3932=ADVANCED_FACE('',(#635,#503),#553,.T.);
#3933=ADVANCED_FACE('',(#636),#3799,.T.);
#3934=ADVANCED_FACE('',(#637),#554,.T.);
#3935=ADVANCED_FACE('',(#638),#3800,.T.);
#3936=ADVANCED_FACE('',(#639),#3801,.T.);
#3937=ADVANCED_FACE('',(#640),#3802,.F.);
#3938=ADVANCED_FACE('',(#641),#555,.T.);
#3939=ADVANCED_FACE('',(#642),#3803,.F.);
#3940=ADVANCED_FACE('',(#643),#556,.T.);
#3941=ADVANCED_FACE('',(#644),#3804,.F.);
#3942=ADVANCED_FACE('',(#645),#557,.T.);
#3943=ADVANCED_FACE('',(#646),#3805,.F.);
#3944=ADVANCED_FACE('',(#647),#558,.T.);
#3945=ADVANCED_FACE('',(#648),#559,.T.);
#3946=ADVANCED_FACE('',(#649),#560,.T.);
#3947=ADVANCED_FACE('',(#650,#504),#561,.F.);
#3948=ADVANCED_FACE('',(#651),#3806,.T.);
#3949=ADVANCED_FACE('',(#652),#562,.T.);
#3950=ADVANCED_FACE('',(#653,#505),#563,.T.);
#3951=ADVANCED_FACE('',(#654),#3807,.T.);
#3952=ADVANCED_FACE('',(#655),#564,.T.);
#3953=ADVANCED_FACE('',(#656),#3808,.T.);
#3954=ADVANCED_FACE('',(#657),#3809,.T.);
#3955=ADVANCED_FACE('',(#658),#3810,.F.);
#3956=ADVANCED_FACE('',(#659),#565,.T.);
#3957=ADVANCED_FACE('',(#660),#3811,.F.);
#3958=ADVANCED_FACE('',(#661),#566,.T.);
#3959=ADVANCED_FACE('',(#662),#3812,.F.);
#3960=ADVANCED_FACE('',(#663),#567,.T.);
#3961=ADVANCED_FACE('',(#664),#3813,.F.);
#3962=ADVANCED_FACE('',(#665),#568,.T.);
#3963=ADVANCED_FACE('',(#666),#569,.T.);
#3964=ADVANCED_FACE('',(#667),#570,.T.);
#3965=ADVANCED_FACE('',(#668,#506),#571,.F.);
#3966=ADVANCED_FACE('',(#669),#3814,.F.);
#3967=ADVANCED_FACE('',(#670),#3815,.F.);
#3968=ADVANCED_FACE('',(#671),#3816,.F.);
#3969=ADVANCED_FACE('',(#672),#3817,.F.);
#3970=ADVANCED_FACE('',(#673),#572,.T.);
#3971=ADVANCED_FACE('',(#674),#573,.T.);
#3972=ADVANCED_FACE('',(#675),#574,.T.);
#3973=ADVANCED_FACE('',(#676),#575,.T.);
#3974=ADVANCED_FACE('',(#677,#507,#508,#509,#510),#576,.T.);
#3975=ADVANCED_FACE('',(#678,#511,#512,#513,#514),#577,.F.);
#3976=ADVANCED_FACE('',(#679),#3818,.F.);
#3977=ADVANCED_FACE('',(#680),#3819,.F.);
#3978=ADVANCED_FACE('',(#681),#3820,.F.);
#3979=ADVANCED_FACE('',(#682),#3821,.F.);
#3980=ADVANCED_FACE('',(#683),#578,.T.);
#3981=ADVANCED_FACE('',(#684),#579,.T.);
#3982=ADVANCED_FACE('',(#685),#580,.T.);
#3983=ADVANCED_FACE('',(#686),#581,.T.);
#3984=ADVANCED_FACE('',(#687,#515,#516,#517,#518),#582,.T.);
#3985=ADVANCED_FACE('',(#688,#519,#520,#521,#522),#583,.F.);
#3986=ADVANCED_FACE('',(#689),#584,.T.);
#3987=ADVANCED_FACE('',(#690),#585,.T.);
#3988=ADVANCED_FACE('',(#691),#586,.T.);
#3989=ADVANCED_FACE('',(#692),#587,.T.);
#3990=ADVANCED_FACE('',(#693),#588,.T.);
#3991=ADVANCED_FACE('',(#694),#589,.F.);
#3992=ADVANCED_FACE('',(#695),#590,.T.);
#3993=ADVANCED_FACE('',(#696),#591,.T.);
#3994=ADVANCED_FACE('',(#697),#592,.T.);
#3995=ADVANCED_FACE('',(#698),#593,.T.);
#3996=ADVANCED_FACE('',(#699),#594,.T.);
#3997=ADVANCED_FACE('',(#700),#595,.F.);
#3998=ADVANCED_FACE('',(#701),#3822,.F.);
#3999=ADVANCED_FACE('',(#702),#3823,.F.);
#4000=ADVANCED_FACE('',(#703),#3824,.F.);
#4001=ADVANCED_FACE('',(#704),#3825,.F.);
#4002=ADVANCED_FACE('',(#705,#523,#524,#525,#526),#596,.T.);
#4003=ADVANCED_FACE('',(#706),#597,.T.);
#4004=ADVANCED_FACE('',(#707,#527,#528,#529,#530),#598,.T.);
#4005=ADVANCED_FACE('',(#708),#599,.T.);
#4006=ADVANCED_FACE('',(#709),#600,.T.);
#4007=ADVANCED_FACE('',(#710),#601,.F.);
#4008=ADVANCED_FACE('',(#711),#3826,.F.);
#4009=ADVANCED_FACE('',(#712),#3827,.F.);
#4010=ADVANCED_FACE('',(#713),#3828,.F.);
#4011=ADVANCED_FACE('',(#714),#3829,.F.);
#4012=ADVANCED_FACE('',(#715),#3830,.F.);
#4013=ADVANCED_FACE('',(#716),#3831,.F.);
#4014=ADVANCED_FACE('',(#717),#3832,.F.);
#4015=ADVANCED_FACE('',(#718),#3833,.F.);
#4016=ADVANCED_FACE('',(#719),#3834,.F.);
#4017=ADVANCED_FACE('',(#720),#3835,.F.);
#4018=ADVANCED_FACE('',(#721),#3836,.F.);
#4019=ADVANCED_FACE('',(#722),#3837,.F.);
#4020=ADVANCED_FACE('',(#723),#3838,.F.);
#4021=ADVANCED_FACE('',(#724),#3839,.F.);
#4022=ADVANCED_FACE('',(#725),#3840,.F.);
#4023=ADVANCED_FACE('',(#726),#3841,.F.);
#4024=ADVANCED_FACE('',(#727),#3842,.F.);
#4025=ADVANCED_FACE('',(#728),#3843,.F.);
#4026=ADVANCED_FACE('',(#729),#3844,.F.);
#4027=ADVANCED_FACE('',(#730),#3845,.F.);
#4028=ADVANCED_FACE('',(#731),#3846,.F.);
#4029=ADVANCED_FACE('',(#732),#3847,.F.);
#4030=ADVANCED_FACE('',(#733),#3848,.F.);
#4031=ADVANCED_FACE('',(#734),#3849,.F.);
#4032=ADVANCED_FACE('',(#735),#3850,.F.);
#4033=ADVANCED_FACE('',(#736),#3851,.F.);
#4034=ADVANCED_FACE('',(#737),#3852,.F.);
#4035=ADVANCED_FACE('',(#738),#3853,.F.);
#4036=ADVANCED_FACE('',(#739),#3854,.F.);
#4037=ADVANCED_FACE('',(#740),#3855,.F.);
#4038=ADVANCED_FACE('',(#741),#3856,.F.);
#4039=ADVANCED_FACE('',(#742),#3857,.F.);
#4040=ADVANCED_FACE('',(#743),#3858,.F.);
#4041=ADVANCED_FACE('',(#744),#3859,.F.);
#4042=ADVANCED_FACE('',(#745),#3860,.F.);
#4043=ADVANCED_FACE('',(#746),#3861,.F.);
#4044=ADVANCED_FACE('',(#747),#3862,.F.);
#4045=ADVANCED_FACE('',(#748),#3863,.F.);
#4046=ADVANCED_FACE('',(#749),#3864,.F.);
#4047=ADVANCED_FACE('',(#750),#3865,.F.);
#4048=ADVANCED_FACE('',(#751),#3866,.F.);
#4049=ADVANCED_FACE('',(#752),#3867,.F.);
#4050=ADVANCED_FACE('',(#753),#3868,.F.);
#4051=ADVANCED_FACE('',(#754),#3869,.F.);
#4052=ADVANCED_FACE('',(#755),#3870,.F.);
#4053=ADVANCED_FACE('',(#756),#3871,.F.);
#4054=ADVANCED_FACE('',(#757),#3872,.F.);
#4055=ADVANCED_FACE('',(#758),#3873,.F.);
#4056=ADVANCED_FACE('',(#759),#3874,.F.);
#4057=ADVANCED_FACE('',(#760),#3875,.F.);
#4058=ADVANCED_FACE('',(#761),#3876,.F.);
#4059=ADVANCED_FACE('',(#762),#3877,.F.);
#4060=ADVANCED_FACE('',(#763),#3878,.F.);
#4061=ADVANCED_FACE('',(#764),#3879,.F.);
#4062=ADVANCED_FACE('',(#765),#3880,.F.);
#4063=ADVANCED_FACE('',(#766),#3881,.F.);
#4064=ADVANCED_FACE('',(#767),#3882,.F.);
#4065=ADVANCED_FACE('',(#768),#3883,.F.);
#4066=ADVANCED_FACE('',(#769),#3884,.F.);
#4067=ADVANCED_FACE('',(#770),#3885,.F.);
#4068=ADVANCED_FACE('',(#771),#3886,.F.);
#4069=ADVANCED_FACE('',(#772),#3887,.F.);
#4070=ADVANCED_FACE('',(#773),#3888,.F.);
#4071=ADVANCED_FACE('',(#774),#3889,.F.);
#4072=ADVANCED_FACE('',(#775),#3890,.F.);
#4073=ADVANCED_FACE('',(#776),#3891,.F.);
#4074=ADVANCED_FACE('',(#777),#3892,.F.);
#4075=ADVANCED_FACE('',(#778),#3893,.F.);
#4076=ADVANCED_FACE('',(#779),#3894,.F.);
#4077=ADVANCED_FACE('',(#780),#3895,.F.);
#4078=ADVANCED_FACE('',(#781),#3896,.F.);
#4079=ADVANCED_FACE('',(#782),#3897,.F.);
#4080=ADVANCED_FACE('',(#783),#3898,.F.);
#4081=ADVANCED_FACE('',(#784),#3899,.F.);
#4082=ADVANCED_FACE('',(#785),#3900,.F.);
#4083=ADVANCED_FACE('',(#786),#3901,.F.);
#4084=ADVANCED_FACE('',(#787),#3902,.F.);
#4085=ADVANCED_FACE('',(#788),#3903,.F.);
#4086=ADVANCED_FACE('',(#789),#3904,.F.);
#4087=ADVANCED_FACE('',(#790),#3905,.F.);
#4088=ADVANCED_FACE('',(#791),#3906,.F.);
#4089=ADVANCED_FACE('',(#792),#239,.F.);
#4090=ADVANCED_FACE('',(#793),#240,.F.);
#4091=ADVANCED_FACE('',(#794,#531,#532,#533,#534),#602,.T.);
#4092=ADVANCED_FACE('',(#795),#3907,.F.);
#4093=ADVANCED_FACE('',(#796),#241,.F.);
#4094=ADVANCED_FACE('',(#797),#242,.F.);
#4095=ADVANCED_FACE('',(#798),#3908,.F.);
#4096=ADVANCED_FACE('',(#799),#243,.F.);
#4097=ADVANCED_FACE('',(#800),#244,.F.);
#4098=ADVANCED_FACE('',(#801),#3909,.F.);
#4099=ADVANCED_FACE('',(#802),#245,.F.);
#4100=ADVANCED_FACE('',(#803),#246,.F.);
#4101=ADVANCED_FACE('',(#804),#3910,.F.);
#4102=ADVANCED_FACE('',(#805),#3911,.F.);
#4103=ADVANCED_FACE('',(#806),#3912,.F.);
#4104=ADVANCED_FACE('',(#807),#3913,.F.);
#4105=ADVANCED_FACE('',(#808),#603,.T.);
#4106=ADVANCED_FACE('',(#809),#604,.T.);
#4107=ADVANCED_FACE('',(#810),#605,.T.);
#4108=ADVANCED_FACE('',(#811),#606,.T.);
#4109=ADVANCED_FACE('',(#812,#535,#536,#537,#538),#607,.F.);
#4110=ADVANCED_FACE('',(#813),#608,.T.);
#4111=ADVANCED_FACE('',(#814),#609,.T.);
#4112=ADVANCED_FACE('',(#815),#610,.T.);
#4113=ADVANCED_FACE('',(#816),#611,.T.);
#4114=ADVANCED_FACE('',(#817),#612,.T.);
#4115=ADVANCED_FACE('',(#818),#613,.F.);
#4116=ADVANCED_FACE('',(#819),#3914,.F.);
#4117=ADVANCED_FACE('',(#820),#3915,.T.);
#4118=ADVANCED_FACE('',(#821,#539),#614,.T.);
#4119=ADVANCED_FACE('',(#822,#540),#615,.F.);
#4120=ADVANCED_FACE('',(#823),#3916,.F.);
#4121=ADVANCED_FACE('',(#824),#3917,.T.);
#4122=ADVANCED_FACE('',(#825,#541),#616,.T.);
#4123=ADVANCED_FACE('',(#826,#542),#617,.F.);
#4124=ADVANCED_FACE('',(#827),#3918,.T.);
#4125=ADVANCED_FACE('',(#828,#543),#618,.F.);
#4126=ADVANCED_FACE('',(#829,#544),#619,.F.);
#4127=ADVANCED_FACE('',(#830),#3919,.T.);
#4128=ADVANCED_FACE('',(#831,#545),#620,.T.);
#4129=ADVANCED_FACE('',(#832),#3920,.T.);
#4130=ADVANCED_FACE('',(#833),#621,.F.);
#4131=ADVANCED_FACE('',(#834),#3921,.T.);
#4132=ADVANCED_FACE('',(#835),#622,.T.);
#4133=ADVANCED_FACE('',(#836),#623,.F.);
#4134=ADVANCED_FACE('',(#837),#624,.F.);
#4135=ADVANCED_FACE('',(#838),#625,.F.);
#4136=ADVANCED_FACE('',(#839),#3922,.F.);
#4137=ADVANCED_FACE('',(#840),#3923,.T.);
#4138=ADVANCED_FACE('',(#841),#626,.T.);
#4139=ADVANCED_FACE('',(#842),#3924,.F.);
#4140=ADVANCED_FACE('',(#843),#3925,.T.);
#4141=ADVANCED_FACE('',(#844,#546),#627,.T.);
#4142=ADVANCED_FACE('',(#845,#547),#628,.F.);
#4143=ADVANCED_FACE('',(#846),#3926,.F.);
#4144=ADVANCED_FACE('',(#847),#3927,.T.);
#4145=ADVANCED_FACE('',(#848,#548),#629,.T.);
#4146=ADVANCED_FACE('',(#849,#549),#630,.F.);
#4147=ADVANCED_FACE('',(#850),#3928,.F.);
#4148=ADVANCED_FACE('',(#851),#3929,.T.);
#4149=ADVANCED_FACE('',(#852,#550),#631,.T.);
#4150=ADVANCED_FACE('',(#853,#551),#632,.F.);
#4151=CLOSED_SHELL('',(#3930,#3931,#3932,#3933,#3934,#3935,#3936,#3937,
#3938,#3939,#3940,#3941,#3942,#3943,#3944,#3945,#3946,#3947));
#4152=CLOSED_SHELL('',(#3948,#3949,#3950,#3951,#3952,#3953,#3954,#3955,
#3956,#3957,#3958,#3959,#3960,#3961,#3962,#3963,#3964,#3965));
#4153=CLOSED_SHELL('',(#3966,#3967,#3968,#3969,#3970,#3971,#3972,#3973,
#3974,#3975));
#4154=CLOSED_SHELL('',(#3976,#3977,#3978,#3979,#3980,#3981,#3982,#3983,
#3984,#3985));
#4155=CLOSED_SHELL('',(#3986,#3987,#3988,#3989,#3990,#3991));
#4156=CLOSED_SHELL('',(#3992,#3993,#3994,#3995,#3996,#3997));
#4157=CLOSED_SHELL('',(#3998,#3999,#4000,#4001,#4002,#4003,#4004,#4005,
#4006,#4007));
#4158=CLOSED_SHELL('',(#4008,#4009,#4010,#4011,#4012,#4013,#4014,#4015,
#4016,#4017,#4018,#4019,#4020,#4021,#4022,#4023,#4024,#4025,#4026,#4027,
#4028,#4029,#4030,#4031,#4032,#4033,#4034,#4035,#4036,#4037,#4038,#4039,
#4040,#4041,#4042,#4043,#4044,#4045,#4046,#4047,#4048,#4049,#4050,#4051,
#4052,#4053,#4054,#4055,#4056,#4057,#4058,#4059,#4060,#4061,#4062,#4063,
#4064,#4065,#4066,#4067,#4068,#4069,#4070,#4071,#4072,#4073,#4074,#4075,
#4076,#4077,#4078,#4079,#4080,#4081,#4082,#4083,#4084,#4085,#4086,#4087,
#4088,#4089,#4090,#4091,#4092,#4093,#4094,#4095,#4096,#4097,#4098,#4099,
#4100,#4101,#4102,#4103,#4104,#4105,#4106,#4107,#4108,#4109));
#4159=CLOSED_SHELL('',(#4110,#4111,#4112,#4113,#4114,#4115));
#4160=CLOSED_SHELL('',(#4116,#4117,#4118,#4119));
#4161=CLOSED_SHELL('',(#4120,#4121,#4122,#4123));
#4162=CLOSED_SHELL('',(#4124,#4125,#4126,#4127,#4128,#4129,#4130,#4131,
#4132));
#4163=CLOSED_SHELL('',(#4133,#4134,#4135,#4136,#4137,#4138));
#4164=CLOSED_SHELL('',(#4139,#4140,#4141,#4142));
#4165=CLOSED_SHELL('',(#4143,#4144,#4145,#4146));
#4166=CLOSED_SHELL('',(#4147,#4148,#4149,#4150));
#4167=DERIVED_UNIT_ELEMENT(#4199,1.);
#4168=DERIVED_UNIT_ELEMENT(#13233,-3.);
#4169=DERIVED_UNIT_ELEMENT(#4199,1.);
#4170=DERIVED_UNIT_ELEMENT(#13233,-3.);
#4171=DERIVED_UNIT_ELEMENT(#4199,1.);
#4172=DERIVED_UNIT_ELEMENT(#13233,-3.);
#4173=DERIVED_UNIT_ELEMENT(#4199,1.);
#4174=DERIVED_UNIT_ELEMENT(#13233,-3.);
#4175=DERIVED_UNIT_ELEMENT(#4199,1.);
#4176=DERIVED_UNIT_ELEMENT(#13233,-3.);
#4177=DERIVED_UNIT_ELEMENT(#4199,1.);
#4178=DERIVED_UNIT_ELEMENT(#13233,-3.);
#4179=DERIVED_UNIT_ELEMENT(#4199,1.);
#4180=DERIVED_UNIT_ELEMENT(#13233,-3.);
#4181=DERIVED_UNIT_ELEMENT(#4199,1.);
#4182=DERIVED_UNIT_ELEMENT(#13233,-3.);
#4183=DERIVED_UNIT_ELEMENT(#4199,1.);
#4184=DERIVED_UNIT_ELEMENT(#13233,-3.);
#4185=DERIVED_UNIT_ELEMENT(#4199,1.);
#4186=DERIVED_UNIT_ELEMENT(#13233,-3.);
#4187=DERIVED_UNIT_ELEMENT(#4199,1.);
#4188=DERIVED_UNIT_ELEMENT(#13233,-3.);
#4189=DERIVED_UNIT_ELEMENT(#4199,1.);
#4190=DERIVED_UNIT_ELEMENT(#13233,-3.);
#4191=DERIVED_UNIT_ELEMENT(#4199,1.);
#4192=DERIVED_UNIT_ELEMENT(#13233,-3.);
#4193=DERIVED_UNIT_ELEMENT(#4199,1.);
#4194=DERIVED_UNIT_ELEMENT(#13233,-3.);
#4195=DERIVED_UNIT_ELEMENT(#4199,1.);
#4196=DERIVED_UNIT_ELEMENT(#13233,-3.);
#4197=DERIVED_UNIT_ELEMENT(#4199,1.);
#4198=DERIVED_UNIT_ELEMENT(#13233,-3.);
#4199=(
MASS_UNIT()
NAMED_UNIT(*)
SI_UNIT(.KILO.,.GRAM.)
);
#4200=DERIVED_UNIT((#4167,#4168));
#4201=DERIVED_UNIT((#4169,#4170));
#4202=DERIVED_UNIT((#4171,#4172));
#4203=DERIVED_UNIT((#4173,#4174));
#4204=DERIVED_UNIT((#4175,#4176));
#4205=DERIVED_UNIT((#4177,#4178));
#4206=DERIVED_UNIT((#4179,#4180));
#4207=DERIVED_UNIT((#4181,#4182));
#4208=DERIVED_UNIT((#4183,#4184));
#4209=DERIVED_UNIT((#4185,#4186));
#4210=DERIVED_UNIT((#4187,#4188));
#4211=DERIVED_UNIT((#4189,#4190));
#4212=DERIVED_UNIT((#4191,#4192));
#4213=DERIVED_UNIT((#4193,#4194));
#4214=DERIVED_UNIT((#4195,#4196));
#4215=DERIVED_UNIT((#4197,#4198));
#4216=MEASURE_REPRESENTATION_ITEM('density measure',
POSITIVE_RATIO_MEASURE(2700.),#4200);
#4217=MEASURE_REPRESENTATION_ITEM('density measure',
POSITIVE_RATIO_MEASURE(2700.),#4201);
#4218=MEASURE_REPRESENTATION_ITEM('density measure',
POSITIVE_RATIO_MEASURE(2700.),#4202);
#4219=MEASURE_REPRESENTATION_ITEM('density measure',
POSITIVE_RATIO_MEASURE(1200.),#4203);
#4220=MEASURE_REPRESENTATION_ITEM('density measure',
POSITIVE_RATIO_MEASURE(2700.),#4204);
#4221=MEASURE_REPRESENTATION_ITEM('density measure',
POSITIVE_RATIO_MEASURE(2700.),#4205);
#4222=MEASURE_REPRESENTATION_ITEM('density measure',
POSITIVE_RATIO_MEASURE(7850.),#4206);
#4223=MEASURE_REPRESENTATION_ITEM('density measure',
POSITIVE_RATIO_MEASURE(7850.),#4207);
#4224=MEASURE_REPRESENTATION_ITEM('density measure',
POSITIVE_RATIO_MEASURE(1425.),#4208);
#4225=MEASURE_REPRESENTATION_ITEM('density measure',
POSITIVE_RATIO_MEASURE(7850.),#4209);
#4226=MEASURE_REPRESENTATION_ITEM('density measure',
POSITIVE_RATIO_MEASURE(8920.),#4210);
#4227=MEASURE_REPRESENTATION_ITEM('density measure',
POSITIVE_RATIO_MEASURE(7850.),#4211);
#4228=MEASURE_REPRESENTATION_ITEM('density measure',
POSITIVE_RATIO_MEASURE(7850.),#4212);
#4229=MEASURE_REPRESENTATION_ITEM('density measure',
POSITIVE_RATIO_MEASURE(7850.),#4213);
#4230=MEASURE_REPRESENTATION_ITEM('density measure',
POSITIVE_RATIO_MEASURE(8920.),#4214);
#4231=MEASURE_REPRESENTATION_ITEM('density measure',
POSITIVE_RATIO_MEASURE(7850.),#4215);
#4232=PROPERTY_DEFINITION_REPRESENTATION(#4312,#4264);
#4233=PROPERTY_DEFINITION_REPRESENTATION(#4313,#4265);
#4234=PROPERTY_DEFINITION_REPRESENTATION(#4314,#4266);
#4235=PROPERTY_DEFINITION_REPRESENTATION(#4315,#4267);
#4236=PROPERTY_DEFINITION_REPRESENTATION(#4316,#4268);
#4237=PROPERTY_DEFINITION_REPRESENTATION(#4317,#4269);
#4238=PROPERTY_DEFINITION_REPRESENTATION(#4318,#4270);
#4239=PROPERTY_DEFINITION_REPRESENTATION(#4319,#4271);
#4240=PROPERTY_DEFINITION_REPRESENTATION(#4320,#4272);
#4241=PROPERTY_DEFINITION_REPRESENTATION(#4321,#4273);
#4242=PROPERTY_DEFINITION_REPRESENTATION(#4322,#4274);
#4243=PROPERTY_DEFINITION_REPRESENTATION(#4323,#4275);
#4244=PROPERTY_DEFINITION_REPRESENTATION(#4324,#4276);
#4245=PROPERTY_DEFINITION_REPRESENTATION(#4325,#4277);
#4246=PROPERTY_DEFINITION_REPRESENTATION(#4326,#4278);
#4247=PROPERTY_DEFINITION_REPRESENTATION(#4327,#4279);
#4248=PROPERTY_DEFINITION_REPRESENTATION(#4328,#4280);
#4249=PROPERTY_DEFINITION_REPRESENTATION(#4329,#4281);
#4250=PROPERTY_DEFINITION_REPRESENTATION(#4330,#4282);
#4251=PROPERTY_DEFINITION_REPRESENTATION(#4331,#4283);
#4252=PROPERTY_DEFINITION_REPRESENTATION(#4332,#4284);
#4253=PROPERTY_DEFINITION_REPRESENTATION(#4333,#4285);
#4254=PROPERTY_DEFINITION_REPRESENTATION(#4334,#4286);
#4255=PROPERTY_DEFINITION_REPRESENTATION(#4335,#4287);
#4256=PROPERTY_DEFINITION_REPRESENTATION(#4336,#4288);
#4257=PROPERTY_DEFINITION_REPRESENTATION(#4337,#4289);
#4258=PROPERTY_DEFINITION_REPRESENTATION(#4338,#4290);
#4259=PROPERTY_DEFINITION_REPRESENTATION(#4339,#4291);
#4260=PROPERTY_DEFINITION_REPRESENTATION(#4340,#4292);
#4261=PROPERTY_DEFINITION_REPRESENTATION(#4341,#4293);
#4262=PROPERTY_DEFINITION_REPRESENTATION(#4342,#4294);
#4263=PROPERTY_DEFINITION_REPRESENTATION(#4343,#4295);
#4264=REPRESENTATION('material name',(#4296),#13215);
#4265=REPRESENTATION('density',(#4216),#13215);
#4266=REPRESENTATION('material name',(#4297),#13216);
#4267=REPRESENTATION('density',(#4217),#13216);
#4268=REPRESENTATION('material name',(#4298),#13217);
#4269=REPRESENTATION('density',(#4218),#13217);
#4270=REPRESENTATION('material name',(#4299),#13218);
#4271=REPRESENTATION('density',(#4219),#13218);
#4272=REPRESENTATION('material name',(#4300),#13219);
#4273=REPRESENTATION('density',(#4220),#13219);
#4274=REPRESENTATION('material name',(#4301),#13220);
#4275=REPRESENTATION('density',(#4221),#13220);
#4276=REPRESENTATION('material name',(#4302),#13221);
#4277=REPRESENTATION('density',(#4222),#13221);
#4278=REPRESENTATION('material name',(#4303),#13222);
#4279=REPRESENTATION('density',(#4223),#13222);
#4280=REPRESENTATION('material name',(#4304),#13223);
#4281=REPRESENTATION('density',(#4224),#13223);
#4282=REPRESENTATION('material name',(#4305),#13224);
#4283=REPRESENTATION('density',(#4225),#13224);
#4284=REPRESENTATION('material name',(#4306),#13225);
#4285=REPRESENTATION('density',(#4226),#13225);
#4286=REPRESENTATION('material name',(#4307),#13226);
#4287=REPRESENTATION('density',(#4227),#13226);
#4288=REPRESENTATION('material name',(#4308),#13227);
#4289=REPRESENTATION('density',(#4228),#13227);
#4290=REPRESENTATION('material name',(#4309),#13228);
#4291=REPRESENTATION('density',(#4229),#13228);
#4292=REPRESENTATION('material name',(#4310),#13229);
#4293=REPRESENTATION('density',(#4230),#13229);
#4294=REPRESENTATION('material name',(#4311),#13230);
#4295=REPRESENTATION('density',(#4231),#13230);
#4296=DESCRIPTIVE_REPRESENTATION_ITEM('Aluminum 6061','Aluminum 6061');
#4297=DESCRIPTIVE_REPRESENTATION_ITEM('Aluminum 6061','Aluminum 6061');
#4298=DESCRIPTIVE_REPRESENTATION_ITEM('Aluminum 6061','Aluminum 6061');
#4299=DESCRIPTIVE_REPRESENTATION_ITEM('Rubber, Nitrile',
'Rubber, Nitrile');
#4300=DESCRIPTIVE_REPRESENTATION_ITEM('Aluminum 6061','Aluminum 6061');
#4301=DESCRIPTIVE_REPRESENTATION_ITEM('Aluminum 6061','Aluminum 6061');
#4302=DESCRIPTIVE_REPRESENTATION_ITEM('Steel','Steel');
#4303=DESCRIPTIVE_REPRESENTATION_ITEM('Steel','Steel');
#4304=DESCRIPTIVE_REPRESENTATION_ITEM('Acetal Resin, White',
'Acetal Resin, White');
#4305=DESCRIPTIVE_REPRESENTATION_ITEM('Steel','Steel');
#4306=DESCRIPTIVE_REPRESENTATION_ITEM('Copper, Alloy','Copper, Alloy');
#4307=DESCRIPTIVE_REPRESENTATION_ITEM('Steel','Steel');
#4308=DESCRIPTIVE_REPRESENTATION_ITEM('Steel','Steel');
#4309=DESCRIPTIVE_REPRESENTATION_ITEM('Steel','Steel');
#4310=DESCRIPTIVE_REPRESENTATION_ITEM('Copper, Alloy','Copper, Alloy');
#4311=DESCRIPTIVE_REPRESENTATION_ITEM('Steel','Steel');
#4312=PROPERTY_DEFINITION('material property','material name',#13346);
#4313=PROPERTY_DEFINITION('material property','density of part',#13346);
#4314=PROPERTY_DEFINITION('material property','material name',#13347);
#4315=PROPERTY_DEFINITION('material property','density of part',#13347);
#4316=PROPERTY_DEFINITION('material property','material name',#13348);
#4317=PROPERTY_DEFINITION('material property','density of part',#13348);
#4318=PROPERTY_DEFINITION('material property','material name',#13349);
#4319=PROPERTY_DEFINITION('material property','density of part',#13349);
#4320=PROPERTY_DEFINITION('material property','material name',#13350);
#4321=PROPERTY_DEFINITION('material property','density of part',#13350);
#4322=PROPERTY_DEFINITION('material property','material name',#13351);
#4323=PROPERTY_DEFINITION('material property','density of part',#13351);
#4324=PROPERTY_DEFINITION('material property','material name',#13352);
#4325=PROPERTY_DEFINITION('material property','density of part',#13352);
#4326=PROPERTY_DEFINITION('material property','material name',#13353);
#4327=PROPERTY_DEFINITION('material property','density of part',#13353);
#4328=PROPERTY_DEFINITION('material property','material name',#13354);
#4329=PROPERTY_DEFINITION('material property','density of part',#13354);
#4330=PROPERTY_DEFINITION('material property','material name',#13355);
#4331=PROPERTY_DEFINITION('material property','density of part',#13355);
#4332=PROPERTY_DEFINITION('material property','material name',#13356);
#4333=PROPERTY_DEFINITION('material property','density of part',#13356);
#4334=PROPERTY_DEFINITION('material property','material name',#13357);
#4335=PROPERTY_DEFINITION('material property','density of part',#13357);
#4336=PROPERTY_DEFINITION('material property','material name',#13358);
#4337=PROPERTY_DEFINITION('material property','density of part',#13358);
#4338=PROPERTY_DEFINITION('material property','material name',#13359);
#4339=PROPERTY_DEFINITION('material property','density of part',#13359);
#4340=PROPERTY_DEFINITION('material property','material name',#13360);
#4341=PROPERTY_DEFINITION('material property','density of part',#13360);
#4342=PROPERTY_DEFINITION('material property','material name',#13361);
#4343=PROPERTY_DEFINITION('material property','density of part',#13361);
#4344=AXIS2_PLACEMENT_3D('',#5779,#4735,#4736);
#4345=AXIS2_PLACEMENT_3D('',#5780,#4737,#4738);
#4346=AXIS2_PLACEMENT_3D('',#5781,#4739,#4740);
#4347=AXIS2_PLACEMENT_3D('',#5784,#4741,#4742);
#4348=AXIS2_PLACEMENT_3D('',#5788,#4744,#4745);
#4349=AXIS2_PLACEMENT_3D('',#5790,#4747,#4748);
#4350=AXIS2_PLACEMENT_3D('',#5796,#4752,#4753);
#4351=AXIS2_PLACEMENT_3D('',#5800,#4755,#4756);
#4352=AXIS2_PLACEMENT_3D('',#5804,#4758,#4759);
#4353=AXIS2_PLACEMENT_3D('',#5807,#4761,#4762);
#4354=AXIS2_PLACEMENT_3D('',#5812,#4764,#4765);
#4355=AXIS2_PLACEMENT_3D('',#5816,#4767,#4768);
#4356=AXIS2_PLACEMENT_3D('',#5820,#4770,#4771);
#4357=AXIS2_PLACEMENT_3D('',#5823,#4773,#4774);
#4358=AXIS2_PLACEMENT_3D('',#5824,#4775,#4776);
#4359=AXIS2_PLACEMENT_3D('',#5828,#4778,#4779);
#4360=AXIS2_PLACEMENT_3D('',#5830,#4781,#4782);
#4361=AXIS2_PLACEMENT_3D('',#5834,#4785,#4786);
#4362=AXIS2_PLACEMENT_3D('',#5836,#4787,#4788);
#4363=AXIS2_PLACEMENT_3D('',#5838,#4790,#4791);
#4364=AXIS2_PLACEMENT_3D('',#5841,#4793,#4794);
#4365=AXIS2_PLACEMENT_3D('',#5842,#4795,#4796);
#4366=AXIS2_PLACEMENT_3D('',#5845,#4797,#4798);
#4367=AXIS2_PLACEMENT_3D('',#5848,#4801,#4802);
#4368=AXIS2_PLACEMENT_3D('',#5852,#4805,#4806);
#4369=AXIS2_PLACEMENT_3D('',#5854,#4807,#4808);
#4370=AXIS2_PLACEMENT_3D('',#5856,#4810,#4811);
#4371=AXIS2_PLACEMENT_3D('',#5860,#4814,#4815);
#4372=AXIS2_PLACEMENT_3D('',#5862,#4816,#4817);
#4373=AXIS2_PLACEMENT_3D('',#5864,#4819,#4820);
#4374=AXIS2_PLACEMENT_3D('',#5868,#4823,#4824);
#4375=AXIS2_PLACEMENT_3D('',#5870,#4825,#4826);
#4376=AXIS2_PLACEMENT_3D('',#5872,#4828,#4829);
#4377=AXIS2_PLACEMENT_3D('',#5874,#4831,#4832);
#4378=AXIS2_PLACEMENT_3D('',#5876,#4834,#4835);
#4379=AXIS2_PLACEMENT_3D('',#5878,#4837,#4838);
#4380=AXIS2_PLACEMENT_3D('',#5879,#4839,#4840);
#4381=AXIS2_PLACEMENT_3D('',#5880,#4841,#4842);
#4382=AXIS2_PLACEMENT_3D('',#5883,#4843,#4844);
#4383=AXIS2_PLACEMENT_3D('',#5887,#4846,#4847);
#4384=AXIS2_PLACEMENT_3D('',#5889,#4849,#4850);
#4385=AXIS2_PLACEMENT_3D('',#5895,#4854,#4855);
#4386=AXIS2_PLACEMENT_3D('',#5899,#4857,#4858);
#4387=AXIS2_PLACEMENT_3D('',#5903,#4860,#4861);
#4388=AXIS2_PLACEMENT_3D('',#5906,#4863,#4864);
#4389=AXIS2_PLACEMENT_3D('',#5911,#4866,#4867);
#4390=AXIS2_PLACEMENT_3D('',#5915,#4869,#4870);
#4391=AXIS2_PLACEMENT_3D('',#5919,#4872,#4873);
#4392=AXIS2_PLACEMENT_3D('',#5922,#4875,#4876);
#4393=AXIS2_PLACEMENT_3D('',#5923,#4877,#4878);
#4394=AXIS2_PLACEMENT_3D('',#5927,#4880,#4881);
#4395=AXIS2_PLACEMENT_3D('',#5929,#4883,#4884);
#4396=AXIS2_PLACEMENT_3D('',#5933,#4887,#4888);
#4397=AXIS2_PLACEMENT_3D('',#5935,#4889,#4890);
#4398=AXIS2_PLACEMENT_3D('',#5937,#4892,#4893);
#4399=AXIS2_PLACEMENT_3D('',#5940,#4895,#4896);
#4400=AXIS2_PLACEMENT_3D('',#5941,#4897,#4898);
#4401=AXIS2_PLACEMENT_3D('',#5944,#4899,#4900);
#4402=AXIS2_PLACEMENT_3D('',#5947,#4903,#4904);
#4403=AXIS2_PLACEMENT_3D('',#5951,#4907,#4908);
#4404=AXIS2_PLACEMENT_3D('',#5953,#4909,#4910);
#4405=AXIS2_PLACEMENT_3D('',#5955,#4912,#4913);
#4406=AXIS2_PLACEMENT_3D('',#5959,#4916,#4917);
#4407=AXIS2_PLACEMENT_3D('',#5961,#4918,#4919);
#4408=AXIS2_PLACEMENT_3D('',#5963,#4921,#4922);
#4409=AXIS2_PLACEMENT_3D('',#5967,#4925,#4926);
#4410=AXIS2_PLACEMENT_3D('',#5969,#4927,#4928);
#4411=AXIS2_PLACEMENT_3D('',#5971,#4930,#4931);
#4412=AXIS2_PLACEMENT_3D('',#5973,#4933,#4934);
#4413=AXIS2_PLACEMENT_3D('',#5975,#4936,#4937);
#4414=AXIS2_PLACEMENT_3D('',#5977,#4939,#4940);
#4415=AXIS2_PLACEMENT_3D('',#5978,#4941,#4942);
#4416=AXIS2_PLACEMENT_3D('',#5979,#4943,#4944);
#4417=AXIS2_PLACEMENT_3D('',#5981,#4945,#4946);
#4418=AXIS2_PLACEMENT_3D('',#5984,#4948,#4949);
#4419=AXIS2_PLACEMENT_3D('',#5985,#4950,#4951);
#4420=AXIS2_PLACEMENT_3D('',#5987,#4952,#4953);
#4421=AXIS2_PLACEMENT_3D('',#5990,#4955,#4956);
#4422=AXIS2_PLACEMENT_3D('',#5991,#4957,#4958);
#4423=AXIS2_PLACEMENT_3D('',#5993,#4959,#4960);
#4424=AXIS2_PLACEMENT_3D('',#5996,#4962,#4963);
#4425=AXIS2_PLACEMENT_3D('',#5997,#4964,#4965);
#4426=AXIS2_PLACEMENT_3D('',#5999,#4966,#4967);
#4427=AXIS2_PLACEMENT_3D('',#6002,#4969,#4970);
#4428=AXIS2_PLACEMENT_3D('',#6003,#4971,#4972);
#4429=AXIS2_PLACEMENT_3D('',#6012,#4977,#4978);
#4430=AXIS2_PLACEMENT_3D('',#6018,#4982,#4983);
#4431=AXIS2_PLACEMENT_3D('',#6024,#4987,#4988);
#4432=AXIS2_PLACEMENT_3D('',#6027,#4991,#4992);
#4433=AXIS2_PLACEMENT_3D('',#6028,#4993,#4994);
#4434=AXIS2_PLACEMENT_3D('',#6029,#4995,#4996);
#4435=AXIS2_PLACEMENT_3D('',#6030,#4997,#4998);
#4436=AXIS2_PLACEMENT_3D('',#6032,#4999,#5000);
#4437=AXIS2_PLACEMENT_3D('',#6035,#5002,#5003);
#4438=AXIS2_PLACEMENT_3D('',#6036,#5004,#5005);
#4439=AXIS2_PLACEMENT_3D('',#6038,#5006,#5007);
#4440=AXIS2_PLACEMENT_3D('',#6041,#5009,#5010);
#4441=AXIS2_PLACEMENT_3D('',#6042,#5011,#5012);
#4442=AXIS2_PLACEMENT_3D('',#6044,#5013,#5014);
#4443=AXIS2_PLACEMENT_3D('',#6047,#5016,#5017);
#4444=AXIS2_PLACEMENT_3D('',#6048,#5018,#5019);
#4445=AXIS2_PLACEMENT_3D('',#6050,#5020,#5021);
#4446=AXIS2_PLACEMENT_3D('',#6053,#5023,#5024);
#4447=AXIS2_PLACEMENT_3D('',#6054,#5025,#5026);
#4448=AXIS2_PLACEMENT_3D('',#6063,#5031,#5032);
#4449=AXIS2_PLACEMENT_3D('',#6069,#5036,#5037);
#4450=AXIS2_PLACEMENT_3D('',#6075,#5041,#5042);
#4451=AXIS2_PLACEMENT_3D('',#6078,#5045,#5046);
#4452=AXIS2_PLACEMENT_3D('',#6079,#5047,#5048);
#4453=AXIS2_PLACEMENT_3D('',#6080,#5049,#5050);
#4454=AXIS2_PLACEMENT_3D('',#6081,#5051,#5052);
#4455=AXIS2_PLACEMENT_3D('',#6090,#5057,#5058);
#4456=AXIS2_PLACEMENT_3D('',#6096,#5062,#5063);
#4457=AXIS2_PLACEMENT_3D('',#6102,#5067,#5068);
#4458=AXIS2_PLACEMENT_3D('',#6105,#5071,#5072);
#4459=AXIS2_PLACEMENT_3D('',#6106,#5073,#5074);
#4460=AXIS2_PLACEMENT_3D('',#6107,#5075,#5076);
#4461=AXIS2_PLACEMENT_3D('',#6108,#5077,#5078);
#4462=AXIS2_PLACEMENT_3D('',#6117,#5083,#5084);
#4463=AXIS2_PLACEMENT_3D('',#6123,#5088,#5089);
#4464=AXIS2_PLACEMENT_3D('',#6129,#5093,#5094);
#4465=AXIS2_PLACEMENT_3D('',#6132,#5097,#5098);
#4466=AXIS2_PLACEMENT_3D('',#6133,#5099,#5100);
#4467=AXIS2_PLACEMENT_3D('',#6134,#5101,#5102);
#4468=AXIS2_PLACEMENT_3D('',#6135,#5103,#5104);
#4469=AXIS2_PLACEMENT_3D('',#6137,#5105,#5106);
#4470=AXIS2_PLACEMENT_3D('',#6140,#5108,#5109);
#4471=AXIS2_PLACEMENT_3D('',#6141,#5110,#5111);
#4472=AXIS2_PLACEMENT_3D('',#6143,#5112,#5113);
#4473=AXIS2_PLACEMENT_3D('',#6146,#5115,#5116);
#4474=AXIS2_PLACEMENT_3D('',#6147,#5117,#5118);
#4475=AXIS2_PLACEMENT_3D('',#6149,#5119,#5120);
#4476=AXIS2_PLACEMENT_3D('',#6152,#5122,#5123);
#4477=AXIS2_PLACEMENT_3D('',#6153,#5124,#5125);
#4478=AXIS2_PLACEMENT_3D('',#6155,#5126,#5127);
#4479=AXIS2_PLACEMENT_3D('',#6158,#5129,#5130);
#4480=AXIS2_PLACEMENT_3D('',#6159,#5131,#5132);
#4481=AXIS2_PLACEMENT_3D('',#6168,#5137,#5138);
#4482=AXIS2_PLACEMENT_3D('',#6174,#5142,#5143);
#4483=AXIS2_PLACEMENT_3D('',#6180,#5147,#5148);
#4484=AXIS2_PLACEMENT_3D('',#6183,#5151,#5152);
#4485=AXIS2_PLACEMENT_3D('',#6184,#5153,#5154);
#4486=AXIS2_PLACEMENT_3D('',#6185,#5155,#5156);
#4487=AXIS2_PLACEMENT_3D('',#6186,#5157,#5158);
#4488=AXIS2_PLACEMENT_3D('',#6196,#5160,#5161);
#4489=AXIS2_PLACEMENT_3D('',#6207,#5162,#5163);
#4490=AXIS2_PLACEMENT_3D('',#6258,#5165,#5166);
#4491=AXIS2_PLACEMENT_3D('',#6309,#5168,#5169);
#4492=AXIS2_PLACEMENT_3D('',#6357,#5171,#5172);
#4493=AXIS2_PLACEMENT_3D('',#6405,#5174,#5175);
#4494=AXIS2_PLACEMENT_3D('',#6456,#5177,#5178);
#4495=AXIS2_PLACEMENT_3D('',#6507,#5180,#5181);
#4496=AXIS2_PLACEMENT_3D('',#6555,#5183,#5184);
#4497=AXIS2_PLACEMENT_3D('',#6606,#5186,#5187);
#4498=AXIS2_PLACEMENT_3D('',#6625,#5189,#5190);
#4499=AXIS2_PLACEMENT_3D('',#6645,#5191,#5192);
#4500=AXIS2_PLACEMENT_3D('',#6655,#5194,#5195);
#4501=AXIS2_PLACEMENT_3D('',#6666,#5196,#5197);
#4502=AXIS2_PLACEMENT_3D('',#6717,#5199,#5200);
#4503=AXIS2_PLACEMENT_3D('',#6768,#5202,#5203);
#4504=AXIS2_PLACEMENT_3D('',#6816,#5205,#5206);
#4505=AXIS2_PLACEMENT_3D('',#6864,#5208,#5209);
#4506=AXIS2_PLACEMENT_3D('',#6915,#5211,#5212);
#4507=AXIS2_PLACEMENT_3D('',#6966,#5214,#5215);
#4508=AXIS2_PLACEMENT_3D('',#7014,#5217,#5218);
#4509=AXIS2_PLACEMENT_3D('',#7065,#5220,#5221);
#4510=AXIS2_PLACEMENT_3D('',#7084,#5223,#5224);
#4511=AXIS2_PLACEMENT_3D('',#7104,#5225,#5226);
#4512=AXIS2_PLACEMENT_3D('',#7114,#5228,#5229);
#4513=AXIS2_PLACEMENT_3D('',#7125,#5230,#5231);
#4514=AXIS2_PLACEMENT_3D('',#7176,#5233,#5234);
#4515=AXIS2_PLACEMENT_3D('',#7227,#5236,#5237);
#4516=AXIS2_PLACEMENT_3D('',#7275,#5239,#5240);
#4517=AXIS2_PLACEMENT_3D('',#7323,#5242,#5243);
#4518=AXIS2_PLACEMENT_3D('',#7374,#5245,#5246);
#4519=AXIS2_PLACEMENT_3D('',#7425,#5248,#5249);
#4520=AXIS2_PLACEMENT_3D('',#7473,#5251,#5252);
#4521=AXIS2_PLACEMENT_3D('',#7524,#5254,#5255);
#4522=AXIS2_PLACEMENT_3D('',#7543,#5257,#5258);
#4523=AXIS2_PLACEMENT_3D('',#7563,#5259,#5260);
#4524=AXIS2_PLACEMENT_3D('',#7573,#5262,#5263);
#4525=AXIS2_PLACEMENT_3D('',#7584,#5264,#5265);
#4526=AXIS2_PLACEMENT_3D('',#7635,#5267,#5268);
#4527=AXIS2_PLACEMENT_3D('',#7686,#5270,#5271);
#4528=AXIS2_PLACEMENT_3D('',#7734,#5273,#5274);
#4529=AXIS2_PLACEMENT_3D('',#7782,#5276,#5277);
#4530=AXIS2_PLACEMENT_3D('',#7833,#5279,#5280);
#4531=AXIS2_PLACEMENT_3D('',#7884,#5282,#5283);
#4532=AXIS2_PLACEMENT_3D('',#7932,#5285,#5286);
#4533=AXIS2_PLACEMENT_3D('',#7983,#5288,#5289);
#4534=AXIS2_PLACEMENT_3D('',#8002,#5291,#5292);
#4535=AXIS2_PLACEMENT_3D('',#8022,#5293,#5294);
#4536=AXIS2_PLACEMENT_3D('',#8036,#5296,#5297);
#4537=AXIS2_PLACEMENT_3D('',#8046,#5298,#5299);
#4538=AXIS2_PLACEMENT_3D('',#8070,#5301,#5302);
#4539=AXIS2_PLACEMENT_3D('',#8095,#5304,#5305);
#4540=AXIS2_PLACEMENT_3D('',#8119,#5307,#5308);
#4541=AXIS2_PLACEMENT_3D('',#8144,#5310,#5311);
#4542=AXIS2_PLACEMENT_3D('',#8168,#5313,#5314);
#4543=AXIS2_PLACEMENT_3D('',#8193,#5316,#5317);
#4544=AXIS2_PLACEMENT_3D('',#8218,#5319,#5320);
#4545=AXIS2_PLACEMENT_3D('',#8242,#5322,#5323);
#4546=AXIS2_PLACEMENT_3D('',#8253,#5325,#5326);
#4547=AXIS2_PLACEMENT_3D('',#8259,#5327,#5328);
#4548=AXIS2_PLACEMENT_3D('',#8273,#5330,#5331);
#4549=AXIS2_PLACEMENT_3D('',#8283,#5332,#5333);
#4550=AXIS2_PLACEMENT_3D('',#8307,#5335,#5336);
#4551=AXIS2_PLACEMENT_3D('',#8332,#5338,#5339);
#4552=AXIS2_PLACEMENT_3D('',#8356,#5341,#5342);
#4553=AXIS2_PLACEMENT_3D('',#8381,#5344,#5345);
#4554=AXIS2_PLACEMENT_3D('',#8405,#5347,#5348);
#4555=AXIS2_PLACEMENT_3D('',#8430,#5350,#5351);
#4556=AXIS2_PLACEMENT_3D('',#8455,#5353,#5354);
#4557=AXIS2_PLACEMENT_3D('',#8479,#5356,#5357);
#4558=AXIS2_PLACEMENT_3D('',#8490,#5359,#5360);
#4559=AXIS2_PLACEMENT_3D('',#8496,#5361,#5362);
#4560=AXIS2_PLACEMENT_3D('',#8510,#5364,#5365);
#4561=AXIS2_PLACEMENT_3D('',#8520,#5366,#5367);
#4562=AXIS2_PLACEMENT_3D('',#8544,#5369,#5370);
#4563=AXIS2_PLACEMENT_3D('',#8569,#5372,#5373);
#4564=AXIS2_PLACEMENT_3D('',#8593,#5375,#5376);
#4565=AXIS2_PLACEMENT_3D('',#8618,#5378,#5379);
#4566=AXIS2_PLACEMENT_3D('',#8642,#5381,#5382);
#4567=AXIS2_PLACEMENT_3D('',#8667,#5384,#5385);
#4568=AXIS2_PLACEMENT_3D('',#8692,#5387,#5388);
#4569=AXIS2_PLACEMENT_3D('',#8716,#5390,#5391);
#4570=AXIS2_PLACEMENT_3D('',#8727,#5393,#5394);
#4571=AXIS2_PLACEMENT_3D('',#8733,#5395,#5396);
#4572=AXIS2_PLACEMENT_3D('',#8747,#5398,#5399);
#4573=AXIS2_PLACEMENT_3D('',#8757,#5400,#5401);
#4574=AXIS2_PLACEMENT_3D('',#8781,#5403,#5404);
#4575=AXIS2_PLACEMENT_3D('',#8806,#5406,#5407);
#4576=AXIS2_PLACEMENT_3D('',#8830,#5409,#5410);
#4577=AXIS2_PLACEMENT_3D('',#8855,#5412,#5413);
#4578=AXIS2_PLACEMENT_3D('',#8879,#5415,#5416);
#4579=AXIS2_PLACEMENT_3D('',#8904,#5418,#5419);
#4580=AXIS2_PLACEMENT_3D('',#8929,#5421,#5422);
#4581=AXIS2_PLACEMENT_3D('',#8953,#5424,#5425);
#4582=AXIS2_PLACEMENT_3D('',#8964,#5427,#5428);
#4583=AXIS2_PLACEMENT_3D('',#8970,#5429,#5430);
#4584=AXIS2_PLACEMENT_3D('',#9965,#5431,#5432);
#4585=AXIS2_PLACEMENT_3D('',#10547,#5437,#5438);
#4586=AXIS2_PLACEMENT_3D('',#11351,#5439,#5440);
#4587=AXIS2_PLACEMENT_3D('',#12155,#5441,#5442);
#4588=AXIS2_PLACEMENT_3D('',#12959,#5443,#5444);
#4589=AXIS2_PLACEMENT_3D('',#12960,#5445,#5446);
#4590=AXIS2_PLACEMENT_3D('',#12961,#5447,#5448);
#4591=AXIS2_PLACEMENT_3D('',#12962,#5449,#5450);
#4592=AXIS2_PLACEMENT_3D('',#12963,#5451,#5452);
#4593=AXIS2_PLACEMENT_3D('',#12969,#5456,#5457);
#4594=AXIS2_PLACEMENT_3D('',#12973,#5460,#5461);
#4595=AXIS2_PLACEMENT_3D('',#12977,#5464,#5465);
#4596=AXIS2_PLACEMENT_3D('',#12979,#5467,#5468);
#4597=AXIS2_PLACEMENT_3D('',#12980,#5469,#5470);
#4598=AXIS2_PLACEMENT_3D('',#12981,#5471,#5472);
#4599=AXIS2_PLACEMENT_3D('',#12990,#5477,#5478);
#4600=AXIS2_PLACEMENT_3D('',#12996,#5482,#5483);
#4601=AXIS2_PLACEMENT_3D('',#13002,#5487,#5488);
#4602=AXIS2_PLACEMENT_3D('',#13005,#5491,#5492);
#4603=AXIS2_PLACEMENT_3D('',#13006,#5493,#5494);
#4604=AXIS2_PLACEMENT_3D('',#13007,#5495,#5496);
#4605=AXIS2_PLACEMENT_3D('',#13008,#5497,#5498);
#4606=AXIS2_PLACEMENT_3D('',#13010,#5499,#5500);
#4607=AXIS2_PLACEMENT_3D('',#13013,#5502,#5503);
#4608=AXIS2_PLACEMENT_3D('',#13014,#5504,#5505);
#4609=AXIS2_PLACEMENT_3D('',#13016,#5506,#5507);
#4610=AXIS2_PLACEMENT_3D('',#13019,#5509,#5510);
#4611=AXIS2_PLACEMENT_3D('',#13020,#5511,#5512);
#4612=AXIS2_PLACEMENT_3D('',#13021,#5513,#5514);
#4613=AXIS2_PLACEMENT_3D('',#13022,#5515,#5516);
#4614=AXIS2_PLACEMENT_3D('',#13023,#5517,#5518);
#4615=AXIS2_PLACEMENT_3D('',#13025,#5519,#5520);
#4616=AXIS2_PLACEMENT_3D('',#13028,#5522,#5523);
#4617=AXIS2_PLACEMENT_3D('',#13029,#5524,#5525);
#4618=AXIS2_PLACEMENT_3D('',#13031,#5526,#5527);
#4619=AXIS2_PLACEMENT_3D('',#13034,#5529,#5530);
#4620=AXIS2_PLACEMENT_3D('',#13035,#5531,#5532);
#4621=AXIS2_PLACEMENT_3D('',#13036,#5533,#5534);
#4622=AXIS2_PLACEMENT_3D('',#13037,#5535,#5536);
#4623=AXIS2_PLACEMENT_3D('',#13038,#5537,#5538);
#4624=AXIS2_PLACEMENT_3D('',#13040,#5539,#5540);
#4625=AXIS2_PLACEMENT_3D('',#13043,#5542,#5543);
#4626=AXIS2_PLACEMENT_3D('',#13044,#5544,#5545);
#4627=AXIS2_PLACEMENT_3D('',#13046,#5546,#5547);
#4628=AXIS2_PLACEMENT_3D('',#13047,#5548,#5549);
#4629=AXIS2_PLACEMENT_3D('',#13049,#5550,#5551);
#4630=AXIS2_PLACEMENT_3D('',#13050,#5552,#5553);
#4631=AXIS2_PLACEMENT_3D('',#13052,#5554,#5555);
#4632=AXIS2_PLACEMENT_3D('',#13054,#5557,#5558);
#4633=AXIS2_PLACEMENT_3D('',#13056,#5559,#5560);
#4634=AXIS2_PLACEMENT_3D('',#13058,#5561,#5562);
#4635=AXIS2_PLACEMENT_3D('',#13059,#5563,#5564);
#4636=AXIS2_PLACEMENT_3D('',#13062,#5566,#5567);
#4637=AXIS2_PLACEMENT_3D('',#13063,#5568,#5569);
#4638=AXIS2_PLACEMENT_3D('',#13064,#5570,#5571);
#4639=AXIS2_PLACEMENT_3D('',#13066,#5573,#5574);
#4640=AXIS2_PLACEMENT_3D('',#13067,#5575,#5576);
#4641=AXIS2_PLACEMENT_3D('',#13068,#5577,#5578);
#4642=AXIS2_PLACEMENT_3D('',#13077,#5583,#5584);
#4643=AXIS2_PLACEMENT_3D('',#13086,#5589,#5590);
#4644=AXIS2_PLACEMENT_3D('',#13087,#5591,#5592);
#4645=AXIS2_PLACEMENT_3D('',#13088,#5593,#5594);
#4646=AXIS2_PLACEMENT_3D('',#13089,#5595,#5596);
#4647=AXIS2_PLACEMENT_3D('',#13090,#5597,#5598);
#4648=AXIS2_PLACEMENT_3D('',#13091,#5599,#5600);
#4649=AXIS2_PLACEMENT_3D('',#13092,#5601,#5602);
#4650=AXIS2_PLACEMENT_3D('',#13093,#5603,#5604);
#4651=AXIS2_PLACEMENT_3D('',#13094,#5605,#5606);
#4652=AXIS2_PLACEMENT_3D('',#13095,#5607,#5608);
#4653=AXIS2_PLACEMENT_3D('',#13097,#5609,#5610);
#4654=AXIS2_PLACEMENT_3D('',#13100,#5612,#5613);
#4655=AXIS2_PLACEMENT_3D('',#13101,#5614,#5615);
#4656=AXIS2_PLACEMENT_3D('',#13103,#5616,#5617);
#4657=AXIS2_PLACEMENT_3D('',#13106,#5619,#5620);
#4658=AXIS2_PLACEMENT_3D('',#13107,#5621,#5622);
#4659=AXIS2_PLACEMENT_3D('',#13108,#5623,#5624);
#4660=AXIS2_PLACEMENT_3D('',#13109,#5625,#5626);
#4661=AXIS2_PLACEMENT_3D('',#13110,#5627,#5628);
#4662=AXIS2_PLACEMENT_3D('',#13112,#5629,#5630);
#4663=AXIS2_PLACEMENT_3D('',#13115,#5632,#5633);
#4664=AXIS2_PLACEMENT_3D('',#13116,#5634,#5635);
#4665=AXIS2_PLACEMENT_3D('',#13118,#5636,#5637);
#4666=AXIS2_PLACEMENT_3D('',#13121,#5639,#5640);
#4667=AXIS2_PLACEMENT_3D('',#13122,#5641,#5642);
#4668=AXIS2_PLACEMENT_3D('',#13123,#5643,#5644);
#4669=AXIS2_PLACEMENT_3D('',#13124,#5645,#5646);
#4670=AXIS2_PLACEMENT_3D('',#13125,#5647,#5648);
#4671=AXIS2_PLACEMENT_3D('',#13127,#5649,#5650);
#4672=AXIS2_PLACEMENT_3D('',#13130,#5652,#5653);
#4673=AXIS2_PLACEMENT_3D('',#13131,#5654,#5655);
#4674=AXIS2_PLACEMENT_3D('',#13133,#5656,#5657);
#4675=AXIS2_PLACEMENT_3D('',#13136,#5659,#5660);
#4676=AXIS2_PLACEMENT_3D('',#13137,#5661,#5662);
#4677=AXIS2_PLACEMENT_3D('',#13138,#5663,#5664);
#4678=AXIS2_PLACEMENT_3D('',#13139,#5665,#5666);
#4679=AXIS2_PLACEMENT_3D('',#13140,#5667,#5668);
#4680=AXIS2_PLACEMENT_3D('',#13141,#5669,#5670);
#4681=AXIS2_PLACEMENT_3D('',#13142,#5671,#5672);
#4682=AXIS2_PLACEMENT_3D('',#13143,#5673,#5674);
#4683=AXIS2_PLACEMENT_3D('',#13144,#5675,#5676);
#4684=AXIS2_PLACEMENT_3D('',#13145,#5677,#5678);
#4685=AXIS2_PLACEMENT_3D('',#13146,#5679,#5680);
#4686=AXIS2_PLACEMENT_3D('',#13147,#5681,#5682);
#4687=AXIS2_PLACEMENT_3D('',#13148,#5683,#5684);
#4688=AXIS2_PLACEMENT_3D('',#13149,#5685,#5686);
#4689=AXIS2_PLACEMENT_3D('',#13150,#5687,#5688);
#4690=AXIS2_PLACEMENT_3D('',#13151,#5689,#5690);
#4691=AXIS2_PLACEMENT_3D('',#13152,#5691,#5692);
#4692=AXIS2_PLACEMENT_3D('',#13153,#5693,#5694);
#4693=AXIS2_PLACEMENT_3D('',#13154,#5695,#5696);
#4694=AXIS2_PLACEMENT_3D('',#13155,#5697,#5698);
#4695=AXIS2_PLACEMENT_3D('',#13156,#5699,#5700);
#4696=AXIS2_PLACEMENT_3D('',#13157,#5701,#5702);
#4697=AXIS2_PLACEMENT_3D('',#13158,#5703,#5704);
#4698=AXIS2_PLACEMENT_3D('',#13159,#5705,#5706);
#4699=AXIS2_PLACEMENT_3D('',#13160,#5707,#5708);
#4700=AXIS2_PLACEMENT_3D('',#13161,#5709,#5710);
#4701=AXIS2_PLACEMENT_3D('',#13162,#5711,#5712);
#4702=AXIS2_PLACEMENT_3D('',#13163,#5713,#5714);
#4703=AXIS2_PLACEMENT_3D('',#13164,#5715,#5716);
#4704=AXIS2_PLACEMENT_3D('',#13165,#5717,#5718);
#4705=AXIS2_PLACEMENT_3D('',#13166,#5719,#5720);
#4706=AXIS2_PLACEMENT_3D('',#13167,#5721,#5722);
#4707=AXIS2_PLACEMENT_3D('',#13168,#5723,#5724);
#4708=AXIS2_PLACEMENT_3D('',#13169,#5725,#5726);
#4709=AXIS2_PLACEMENT_3D('',#13170,#5727,#5728);
#4710=AXIS2_PLACEMENT_3D('',#13171,#5729,#5730);
#4711=AXIS2_PLACEMENT_3D('',#13172,#5731,#5732);
#4712=AXIS2_PLACEMENT_3D('',#13173,#5733,#5734);
#4713=AXIS2_PLACEMENT_3D('',#13174,#5735,#5736);
#4714=AXIS2_PLACEMENT_3D('',#13175,#5737,#5738);
#4715=AXIS2_PLACEMENT_3D('',#13176,#5739,#5740);
#4716=AXIS2_PLACEMENT_3D('',#13177,#5741,#5742);
#4717=AXIS2_PLACEMENT_3D('',#13178,#5743,#5744);
#4718=AXIS2_PLACEMENT_3D('',#13179,#5745,#5746);
#4719=AXIS2_PLACEMENT_3D('',#13180,#5747,#5748);
#4720=AXIS2_PLACEMENT_3D('',#13181,#5749,#5750);
#4721=AXIS2_PLACEMENT_3D('',#13182,#5751,#5752);
#4722=AXIS2_PLACEMENT_3D('',#13183,#5753,#5754);
#4723=AXIS2_PLACEMENT_3D('',#13184,#5755,#5756);
#4724=AXIS2_PLACEMENT_3D('',#13185,#5757,#5758);
#4725=AXIS2_PLACEMENT_3D('',#13186,#5759,#5760);
#4726=AXIS2_PLACEMENT_3D('',#13187,#5761,#5762);
#4727=AXIS2_PLACEMENT_3D('',#13188,#5763,#5764);
#4728=AXIS2_PLACEMENT_3D('',#13189,#5765,#5766);
#4729=AXIS2_PLACEMENT_3D('',#13190,#5767,#5768);
#4730=AXIS2_PLACEMENT_3D('',#13191,#5769,#5770);
#4731=AXIS2_PLACEMENT_3D('',#13192,#5771,#5772);
#4732=AXIS2_PLACEMENT_3D('',#13193,#5773,#5774);
#4733=AXIS2_PLACEMENT_3D('',#13194,#5775,#5776);
#4734=AXIS2_PLACEMENT_3D('',#13195,#5777,#5778);
#4735=DIRECTION('axis',(0.,0.,1.));
#4736=DIRECTION('refdir',(1.,0.,0.));
#4737=DIRECTION('axis',(0.,0.,1.));
#4738=DIRECTION('refdir',(1.,0.,0.));
#4739=DIRECTION('center_axis',(0.,0.,1.));
#4740=DIRECTION('ref_axis',(-0.707106781186546,-0.707106781186549,0.));
#4741=DIRECTION('center_axis',(0.,0.,-1.));
#4742=DIRECTION('ref_axis',(-0.707106781186546,-0.707106781186549,0.));
#4743=DIRECTION('',(0.,0.,-1.));
#4744=DIRECTION('center_axis',(0.,0.,1.));
#4745=DIRECTION('ref_axis',(-0.707106781186546,-0.707106781186549,0.));
#4746=DIRECTION('',(0.,0.,1.));
#4747=DIRECTION('center_axis',(-1.,0.,0.));
#4748=DIRECTION('ref_axis',(0.,-1.,0.));
#4749=DIRECTION('',(0.,-1.,0.));
#4750=DIRECTION('',(0.,0.,1.));
#4751=DIRECTION('',(0.,-1.,0.));
#4752=DIRECTION('center_axis',(0.,0.,1.));
#4753=DIRECTION('ref_axis',(1.,0.,0.));
#4754=DIRECTION('',(1.,0.,0.));
#4755=DIRECTION('center_axis',(0.,0.,-1.));
#4756=DIRECTION('ref_axis',(0.707106781186546,-0.707106781186549,0.));
#4757=DIRECTION('',(0.,1.,0.));
#4758=DIRECTION('center_axis',(0.,0.,-1.));
#4759=DIRECTION('ref_axis',(0.707106781186546,0.707106781186549,0.));
#4760=DIRECTION('',(-1.,0.,0.));
#4761=DIRECTION('center_axis',(0.,0.,-1.));
#4762=DIRECTION('ref_axis',(-0.707106781186546,0.707106781186549,0.));
#4763=DIRECTION('',(0.,1.,0.));
#4764=DIRECTION('center_axis',(0.,0.,1.));
#4765=DIRECTION('ref_axis',(-0.707106781186546,0.707106781186549,0.));
#4766=DIRECTION('',(1.,0.,0.));
#4767=DIRECTION('center_axis',(0.,0.,1.));
#4768=DIRECTION('ref_axis',(0.707106781186546,0.707106781186549,0.));
#4769=DIRECTION('',(0.,-1.,0.));
#4770=DIRECTION('center_axis',(0.,0.,1.));
#4771=DIRECTION('ref_axis',(0.707106781186546,-0.707106781186549,0.));
#4772=DIRECTION('',(-1.,0.,0.));
#4773=DIRECTION('center_axis',(0.,0.,1.));
#4774=DIRECTION('ref_axis',(-0.707106781186546,-0.707106781186549,0.));
#4775=DIRECTION('center_axis',(0.,0.,1.));
#4776=DIRECTION('ref_axis',(0.707106781186546,-0.707106781186549,0.));
#4777=DIRECTION('',(0.,0.,-1.));
#4778=DIRECTION('center_axis',(0.,0.,1.));
#4779=DIRECTION('ref_axis',(0.707106781186546,-0.707106781186549,0.));
#4780=DIRECTION('',(0.,0.,1.));
#4781=DIRECTION('center_axis',(1.,0.,0.));
#4782=DIRECTION('ref_axis',(0.,1.,0.));
#4783=DIRECTION('',(0.,1.,0.));
#4784=DIRECTION('',(0.,0.,-1.));
#4785=DIRECTION('center_axis',(0.,0.,1.));
#4786=DIRECTION('ref_axis',(0.707106781186546,0.707106781186549,0.));
#4787=DIRECTION('center_axis',(0.,0.,1.));
#4788=DIRECTION('ref_axis',(0.707106781186546,0.707106781186549,0.));
#4789=DIRECTION('',(0.,0.,1.));
#4790=DIRECTION('center_axis',(0.,0.,1.));
#4791=DIRECTION('ref_axis',(-0.707106781186546,0.707106781186549,0.));
#4792=DIRECTION('',(0.,0.,-1.));
#4793=DIRECTION('center_axis',(0.,0.,1.));
#4794=DIRECTION('ref_axis',(-0.707106781186546,0.707106781186549,0.));
#4795=DIRECTION('center_axis',(0.,0.,1.));
#4796=DIRECTION('ref_axis',(-0.707106781186546,0.707106781186549,0.));
#4797=DIRECTION('center_axis',(0.,0.,-1.));
#4798=DIRECTION('ref_axis',(-0.707106781186546,0.707106781186549,0.));
#4799=DIRECTION('',(0.,0.,1.));
#4800=DIRECTION('',(0.,0.,-1.));
#4801=DIRECTION('center_axis',(0.,-1.,0.));
#4802=DIRECTION('ref_axis',(1.,0.,0.));
#4803=DIRECTION('',(1.,0.,0.));
#4804=DIRECTION('',(0.,0.,-1.));
#4805=DIRECTION('center_axis',(0.,0.,1.));
#4806=DIRECTION('ref_axis',(0.707106781186546,0.707106781186549,0.));
#4807=DIRECTION('center_axis',(0.,0.,-1.));
#4808=DIRECTION('ref_axis',(0.707106781186546,0.707106781186549,0.));
#4809=DIRECTION('',(0.,0.,1.));
#4810=DIRECTION('center_axis',(-1.,0.,0.));
#4811=DIRECTION('ref_axis',(0.,-1.,0.));
#4812=DIRECTION('',(0.,-1.,0.));
#4813=DIRECTION('',(0.,0.,-1.));
#4814=DIRECTION('center_axis',(0.,0.,1.));
#4815=DIRECTION('ref_axis',(0.707106781186546,-0.707106781186549,0.));
#4816=DIRECTION('center_axis',(0.,0.,-1.));
#4817=DIRECTION('ref_axis',(0.707106781186546,-0.707106781186549,0.));
#4818=DIRECTION('',(0.,0.,1.));
#4819=DIRECTION('center_axis',(0.,1.,0.));
#4820=DIRECTION('ref_axis',(-1.,0.,0.));
#4821=DIRECTION('',(-1.,0.,0.));
#4822=DIRECTION('',(0.,0.,-1.));
#4823=DIRECTION('center_axis',(0.,0.,1.));
#4824=DIRECTION('ref_axis',(-0.707106781186546,-0.707106781186549,0.));
#4825=DIRECTION('center_axis',(0.,0.,-1.));
#4826=DIRECTION('ref_axis',(-0.707106781186546,-0.707106781186549,0.));
#4827=DIRECTION('',(0.,0.,1.));
#4828=DIRECTION('center_axis',(1.,0.,0.));
#4829=DIRECTION('ref_axis',(0.,1.,0.));
#4830=DIRECTION('',(0.,1.,0.));
#4831=DIRECTION('center_axis',(0.,1.,0.));
#4832=DIRECTION('ref_axis',(-1.,0.,0.));
#4833=DIRECTION('',(-1.,0.,0.));
#4834=DIRECTION('center_axis',(0.,-1.,0.));
#4835=DIRECTION('ref_axis',(1.,0.,0.));
#4836=DIRECTION('',(1.,0.,0.));
#4837=DIRECTION('center_axis',(0.,0.,1.));
#4838=DIRECTION('ref_axis',(1.,0.,0.));
#4839=DIRECTION('axis',(0.,0.,1.));
#4840=DIRECTION('refdir',(1.,0.,0.));
#4841=DIRECTION('center_axis',(0.,0.,1.));
#4842=DIRECTION('ref_axis',(-0.707106781186548,-0.707106781186548,0.));
#4843=DIRECTION('center_axis',(0.,0.,-1.));
#4844=DIRECTION('ref_axis',(-0.707106781186548,-0.707106781186548,0.));
#4845=DIRECTION('',(0.,0.,-1.));
#4846=DIRECTION('center_axis',(0.,0.,1.));
#4847=DIRECTION('ref_axis',(-0.707106781186548,-0.707106781186548,0.));
#4848=DIRECTION('',(0.,0.,1.));
#4849=DIRECTION('center_axis',(-1.,0.,0.));
#4850=DIRECTION('ref_axis',(0.,-1.,0.));
#4851=DIRECTION('',(0.,-1.,0.));
#4852=DIRECTION('',(0.,0.,1.));
#4853=DIRECTION('',(0.,-1.,0.));
#4854=DIRECTION('center_axis',(0.,0.,1.));
#4855=DIRECTION('ref_axis',(1.,0.,0.));
#4856=DIRECTION('',(1.,0.,0.));
#4857=DIRECTION('center_axis',(0.,0.,-1.));
#4858=DIRECTION('ref_axis',(0.707106781186548,-0.707106781186548,0.));
#4859=DIRECTION('',(0.,1.,0.));
#4860=DIRECTION('center_axis',(0.,0.,-1.));
#4861=DIRECTION('ref_axis',(0.707106781186548,0.707106781186548,0.));
#4862=DIRECTION('',(-1.,0.,0.));
#4863=DIRECTION('center_axis',(0.,0.,-1.));
#4864=DIRECTION('ref_axis',(-0.707106781186548,0.707106781186548,0.));
#4865=DIRECTION('',(0.,1.,0.));
#4866=DIRECTION('center_axis',(0.,0.,1.));
#4867=DIRECTION('ref_axis',(-0.707106781186548,0.707106781186548,0.));
#4868=DIRECTION('',(1.,0.,0.));
#4869=DIRECTION('center_axis',(0.,0.,1.));
#4870=DIRECTION('ref_axis',(0.707106781186548,0.707106781186548,0.));
#4871=DIRECTION('',(0.,-1.,0.));
#4872=DIRECTION('center_axis',(0.,0.,1.));
#4873=DIRECTION('ref_axis',(0.707106781186548,-0.707106781186548,0.));
#4874=DIRECTION('',(-1.,0.,0.));
#4875=DIRECTION('center_axis',(0.,0.,1.));
#4876=DIRECTION('ref_axis',(-0.707106781186548,-0.707106781186548,0.));
#4877=DIRECTION('center_axis',(0.,0.,1.));
#4878=DIRECTION('ref_axis',(0.707106781186548,-0.707106781186548,0.));
#4879=DIRECTION('',(0.,0.,-1.));
#4880=DIRECTION('center_axis',(0.,0.,1.));
#4881=DIRECTION('ref_axis',(0.707106781186548,-0.707106781186548,0.));
#4882=DIRECTION('',(0.,0.,1.));
#4883=DIRECTION('center_axis',(1.,0.,0.));
#4884=DIRECTION('ref_axis',(0.,1.,0.));
#4885=DIRECTION('',(0.,1.,0.));
#4886=DIRECTION('',(0.,0.,-1.));
#4887=DIRECTION('center_axis',(0.,0.,1.));
#4888=DIRECTION('ref_axis',(0.707106781186548,0.707106781186548,0.));
#4889=DIRECTION('center_axis',(0.,0.,1.));
#4890=DIRECTION('ref_axis',(0.707106781186548,0.707106781186548,0.));
#4891=DIRECTION('',(0.,0.,1.));
#4892=DIRECTION('center_axis',(0.,0.,1.));
#4893=DIRECTION('ref_axis',(-0.707106781186548,0.707106781186548,0.));
#4894=DIRECTION('',(0.,0.,-1.));
#4895=DIRECTION('center_axis',(0.,0.,1.));
#4896=DIRECTION('ref_axis',(-0.707106781186548,0.707106781186548,0.));
#4897=DIRECTION('center_axis',(0.,0.,1.));
#4898=DIRECTION('ref_axis',(-0.707106781186548,0.707106781186548,0.));
#4899=DIRECTION('center_axis',(0.,0.,-1.));
#4900=DIRECTION('ref_axis',(-0.707106781186548,0.707106781186548,0.));
#4901=DIRECTION('',(0.,0.,1.));
#4902=DIRECTION('',(0.,0.,-1.));
#4903=DIRECTION('center_axis',(0.,-1.,0.));
#4904=DIRECTION('ref_axis',(1.,0.,0.));
#4905=DIRECTION('',(1.,0.,0.));
#4906=DIRECTION('',(0.,0.,-1.));
#4907=DIRECTION('center_axis',(0.,0.,1.));
#4908=DIRECTION('ref_axis',(0.707106781186548,0.707106781186548,0.));
#4909=DIRECTION('center_axis',(0.,0.,-1.));
#4910=DIRECTION('ref_axis',(0.707106781186548,0.707106781186548,0.));
#4911=DIRECTION('',(0.,0.,1.));
#4912=DIRECTION('center_axis',(-1.,0.,0.));
#4913=DIRECTION('ref_axis',(0.,-1.,0.));
#4914=DIRECTION('',(0.,-1.,0.));
#4915=DIRECTION('',(0.,0.,-1.));
#4916=DIRECTION('center_axis',(0.,0.,1.));
#4917=DIRECTION('ref_axis',(0.707106781186548,-0.707106781186548,0.));
#4918=DIRECTION('center_axis',(0.,0.,-1.));
#4919=DIRECTION('ref_axis',(0.707106781186548,-0.707106781186548,0.));
#4920=DIRECTION('',(0.,0.,1.));
#4921=DIRECTION('center_axis',(0.,1.,0.));
#4922=DIRECTION('ref_axis',(-1.,0.,0.));
#4923=DIRECTION('',(-1.,0.,0.));
#4924=DIRECTION('',(0.,0.,-1.));
#4925=DIRECTION('center_axis',(0.,0.,1.));
#4926=DIRECTION('ref_axis',(-0.707106781186548,-0.707106781186548,0.));
#4927=DIRECTION('center_axis',(0.,0.,-1.));
#4928=DIRECTION('ref_axis',(-0.707106781186548,-0.707106781186548,0.));
#4929=DIRECTION('',(0.,0.,1.));
#4930=DIRECTION('center_axis',(1.,0.,0.));
#4931=DIRECTION('ref_axis',(0.,1.,0.));
#4932=DIRECTION('',(0.,1.,0.));
#4933=DIRECTION('center_axis',(0.,1.,0.));
#4934=DIRECTION('ref_axis',(-1.,0.,0.));
#4935=DIRECTION('',(-1.,0.,0.));
#4936=DIRECTION('center_axis',(0.,-1.,0.));
#4937=DIRECTION('ref_axis',(1.,0.,0.));
#4938=DIRECTION('',(1.,0.,0.));
#4939=DIRECTION('center_axis',(0.,0.,1.));
#4940=DIRECTION('ref_axis',(1.,0.,0.));
#4941=DIRECTION('axis',(0.,0.,1.));
#4942=DIRECTION('refdir',(1.,0.,0.));
#4943=DIRECTION('center_axis',(0.,0.,-1.));
#4944=DIRECTION('ref_axis',(1.,0.,0.));
#4945=DIRECTION('center_axis',(0.,0.,-1.));
#4946=DIRECTION('ref_axis',(1.,0.,0.));
#4947=DIRECTION('',(0.,0.,-1.));
#4948=DIRECTION('center_axis',(0.,0.,1.));
#4949=DIRECTION('ref_axis',(1.,0.,0.));
#4950=DIRECTION('center_axis',(0.,0.,-1.));
#4951=DIRECTION('ref_axis',(1.,0.,0.));
#4952=DIRECTION('center_axis',(0.,0.,-1.));
#4953=DIRECTION('ref_axis',(1.,0.,0.));
#4954=DIRECTION('',(0.,0.,-1.));
#4955=DIRECTION('center_axis',(0.,0.,1.));
#4956=DIRECTION('ref_axis',(1.,0.,0.));
#4957=DIRECTION('center_axis',(0.,0.,-1.));
#4958=DIRECTION('ref_axis',(1.,0.,0.));
#4959=DIRECTION('center_axis',(0.,0.,-1.));
#4960=DIRECTION('ref_axis',(1.,0.,0.));
#4961=DIRECTION('',(0.,0.,-1.));
#4962=DIRECTION('center_axis',(0.,0.,1.));
#4963=DIRECTION('ref_axis',(1.,0.,0.));
#4964=DIRECTION('center_axis',(0.,0.,-1.));
#4965=DIRECTION('ref_axis',(1.,0.,0.));
#4966=DIRECTION('center_axis',(0.,0.,-1.));
#4967=DIRECTION('ref_axis',(1.,0.,0.));
#4968=DIRECTION('',(0.,0.,-1.));
#4969=DIRECTION('center_axis',(0.,0.,1.));
#4970=DIRECTION('ref_axis',(1.,0.,0.));
#4971=DIRECTION('center_axis',(0.,1.,0.));
#4972=DIRECTION('ref_axis',(-1.,0.,0.));
#4973=DIRECTION('',(1.,0.,0.));
#4974=DIRECTION('',(0.,0.,1.));
#4975=DIRECTION('',(1.,0.,0.));
#4976=DIRECTION('',(0.,0.,-1.));
#4977=DIRECTION('center_axis',(1.,0.,0.));
#4978=DIRECTION('ref_axis',(0.,1.,0.));
#4979=DIRECTION('',(0.,-1.,0.));
#4980=DIRECTION('',(0.,-1.,0.));
#4981=DIRECTION('',(0.,0.,1.));
#4982=DIRECTION('center_axis',(0.,-1.,0.));
#4983=DIRECTION('ref_axis',(1.,0.,0.));
#4984=DIRECTION('',(-1.,0.,0.));
#4985=DIRECTION('',(-1.,0.,0.));
#4986=DIRECTION('',(0.,0.,-1.));
#4987=DIRECTION('center_axis',(-1.,0.,0.));
#4988=DIRECTION('ref_axis',(0.,-1.,0.));
#4989=DIRECTION('',(0.,-1.,0.));
#4990=DIRECTION('',(0.,-1.,0.));
#4991=DIRECTION('center_axis',(0.,0.,1.));
#4992=DIRECTION('ref_axis',(1.,0.,0.));
#4993=DIRECTION('center_axis',(0.,0.,1.));
#4994=DIRECTION('ref_axis',(1.,0.,0.));
#4995=DIRECTION('axis',(0.,0.,1.));
#4996=DIRECTION('refdir',(1.,0.,0.));
#4997=DIRECTION('center_axis',(0.,0.,-1.));
#4998=DIRECTION('ref_axis',(1.,0.,0.));
#4999=DIRECTION('center_axis',(0.,0.,-1.));
#5000=DIRECTION('ref_axis',(1.,0.,0.));
#5001=DIRECTION('',(0.,0.,-1.));
#5002=DIRECTION('center_axis',(0.,0.,1.));
#5003=DIRECTION('ref_axis',(1.,0.,0.));
#5004=DIRECTION('center_axis',(0.,0.,-1.));
#5005=DIRECTION('ref_axis',(1.,0.,0.));
#5006=DIRECTION('center_axis',(0.,0.,-1.));
#5007=DIRECTION('ref_axis',(1.,0.,0.));
#5008=DIRECTION('',(0.,0.,-1.));
#5009=DIRECTION('center_axis',(0.,0.,1.));
#5010=DIRECTION('ref_axis',(1.,0.,0.));
#5011=DIRECTION('center_axis',(0.,0.,-1.));
#5012=DIRECTION('ref_axis',(1.,0.,0.));
#5013=DIRECTION('center_axis',(0.,0.,-1.));
#5014=DIRECTION('ref_axis',(1.,0.,0.));
#5015=DIRECTION('',(0.,0.,-1.));
#5016=DIRECTION('center_axis',(0.,0.,1.));
#5017=DIRECTION('ref_axis',(1.,0.,0.));
#5018=DIRECTION('center_axis',(0.,0.,-1.));
#5019=DIRECTION('ref_axis',(1.,0.,0.));
#5020=DIRECTION('center_axis',(0.,0.,-1.));
#5021=DIRECTION('ref_axis',(1.,0.,0.));
#5022=DIRECTION('',(0.,0.,-1.));
#5023=DIRECTION('center_axis',(0.,0.,1.));
#5024=DIRECTION('ref_axis',(1.,0.,0.));
#5025=DIRECTION('center_axis',(0.,1.,0.));
#5026=DIRECTION('ref_axis',(-1.,0.,0.));
#5027=DIRECTION('',(1.,0.,0.));
#5028=DIRECTION('',(0.,0.,1.));
#5029=DIRECTION('',(1.,0.,0.));
#5030=DIRECTION('',(0.,0.,1.));
#5031=DIRECTION('center_axis',(1.,0.,0.));
#5032=DIRECTION('ref_axis',(0.,1.,0.));
#5033=DIRECTION('',(0.,-1.,0.));
#5034=DIRECTION('',(0.,-1.,0.));
#5035=DIRECTION('',(0.,0.,1.));
#5036=DIRECTION('center_axis',(0.,-1.,0.));
#5037=DIRECTION('ref_axis',(1.,0.,0.));
#5038=DIRECTION('',(-1.,0.,0.));
#5039=DIRECTION('',(-1.,0.,0.));
#5040=DIRECTION('',(0.,0.,-1.));
#5041=DIRECTION('center_axis',(-1.,0.,0.));
#5042=DIRECTION('ref_axis',(0.,-1.,0.));
#5043=DIRECTION('',(0.,-1.,0.));
#5044=DIRECTION('',(0.,-1.,0.));
#5045=DIRECTION('center_axis',(0.,0.,1.));
#5046=DIRECTION('ref_axis',(1.,0.,0.));
#5047=DIRECTION('center_axis',(0.,0.,1.));
#5048=DIRECTION('ref_axis',(1.,0.,0.));
#5049=DIRECTION('axis',(0.,0.,1.));
#5050=DIRECTION('refdir',(1.,0.,0.));
#5051=DIRECTION('center_axis',(0.,1.,0.));
#5052=DIRECTION('ref_axis',(-1.,0.,0.));
#5053=DIRECTION('',(-1.,0.,0.));
#5054=DIRECTION('',(0.,0.,1.));
#5055=DIRECTION('',(-1.,0.,0.));
#5056=DIRECTION('',(0.,0.,1.));
#5057=DIRECTION('center_axis',(1.,0.,0.));
#5058=DIRECTION('ref_axis',(0.,1.,0.));
#5059=DIRECTION('',(0.,1.,0.));
#5060=DIRECTION('',(0.,1.,0.));
#5061=DIRECTION('',(0.,0.,1.));
#5062=DIRECTION('center_axis',(0.,-1.,0.));
#5063=DIRECTION('ref_axis',(1.,0.,0.));
#5064=DIRECTION('',(1.,0.,0.));
#5065=DIRECTION('',(1.,0.,0.));
#5066=DIRECTION('',(0.,0.,1.));
#5067=DIRECTION('center_axis',(-1.,0.,0.));
#5068=DIRECTION('ref_axis',(0.,-1.,0.));
#5069=DIRECTION('',(0.,-1.,0.));
#5070=DIRECTION('',(0.,-1.,0.));
#5071=DIRECTION('center_axis',(0.,0.,1.));
#5072=DIRECTION('ref_axis',(1.,0.,0.));
#5073=DIRECTION('center_axis',(0.,0.,1.));
#5074=DIRECTION('ref_axis',(1.,0.,0.));
#5075=DIRECTION('axis',(0.,0.,1.));
#5076=DIRECTION('refdir',(1.,0.,0.));
#5077=DIRECTION('center_axis',(0.,1.,0.));
#5078=DIRECTION('ref_axis',(-1.,0.,0.));
#5079=DIRECTION('',(-1.,0.,0.));
#5080=DIRECTION('',(0.,0.,1.));
#5081=DIRECTION('',(-1.,0.,0.));
#5082=DIRECTION('',(0.,0.,1.));
#5083=DIRECTION('center_axis',(1.,0.,0.));
#5084=DIRECTION('ref_axis',(0.,1.,0.));
#5085=DIRECTION('',(0.,1.,0.));
#5086=DIRECTION('',(0.,1.,0.));
#5087=DIRECTION('',(0.,0.,1.));
#5088=DIRECTION('center_axis',(0.,-1.,0.));
#5089=DIRECTION('ref_axis',(1.,0.,0.));
#5090=DIRECTION('',(1.,0.,0.));
#5091=DIRECTION('',(1.,0.,0.));
#5092=DIRECTION('',(0.,0.,1.));
#5093=DIRECTION('center_axis',(-1.,0.,0.));
#5094=DIRECTION('ref_axis',(0.,-1.,0.));
#5095=DIRECTION('',(0.,-1.,0.));
#5096=DIRECTION('',(0.,-1.,0.));
#5097=DIRECTION('center_axis',(0.,0.,1.));
#5098=DIRECTION('ref_axis',(1.,0.,0.));
#5099=DIRECTION('center_axis',(0.,0.,1.));
#5100=DIRECTION('ref_axis',(1.,0.,0.));
#5101=DIRECTION('axis',(0.,0.,1.));
#5102=DIRECTION('refdir',(1.,0.,0.));
#5103=DIRECTION('center_axis',(0.,-1.,0.));
#5104=DIRECTION('ref_axis',(0.,0.,1.));
#5105=DIRECTION('center_axis',(0.,-1.,0.));
#5106=DIRECTION('ref_axis',(0.,0.,1.));
#5107=DIRECTION('',(0.,-1.,0.));
#5108=DIRECTION('center_axis',(0.,1.,0.));
#5109=DIRECTION('ref_axis',(0.,0.,1.));
#5110=DIRECTION('center_axis',(0.,-1.,0.));
#5111=DIRECTION('ref_axis',(0.,0.,1.));
#5112=DIRECTION('center_axis',(0.,-1.,0.));
#5113=DIRECTION('ref_axis',(0.,0.,1.));
#5114=DIRECTION('',(0.,-1.,0.));
#5115=DIRECTION('center_axis',(0.,1.,0.));
#5116=DIRECTION('ref_axis',(0.,0.,1.));
#5117=DIRECTION('center_axis',(0.,-1.,0.));
#5118=DIRECTION('ref_axis',(0.,0.,1.));
#5119=DIRECTION('center_axis',(0.,-1.,0.));
#5120=DIRECTION('ref_axis',(0.,0.,1.));
#5121=DIRECTION('',(0.,-1.,0.));
#5122=DIRECTION('center_axis',(0.,1.,0.));
#5123=DIRECTION('ref_axis',(0.,0.,1.));
#5124=DIRECTION('center_axis',(0.,-1.,0.));
#5125=DIRECTION('ref_axis',(0.,0.,1.));
#5126=DIRECTION('center_axis',(0.,-1.,0.));
#5127=DIRECTION('ref_axis',(0.,0.,1.));
#5128=DIRECTION('',(0.,-1.,0.));
#5129=DIRECTION('center_axis',(0.,1.,0.));
#5130=DIRECTION('ref_axis',(0.,0.,1.));
#5131=DIRECTION('center_axis',(0.,1.,0.));
#5132=DIRECTION('ref_axis',(-1.,0.,0.));
#5133=DIRECTION('',(-1.,0.,0.));
#5134=DIRECTION('',(0.,0.,1.));
#5135=DIRECTION('',(-1.,0.,0.));
#5136=DIRECTION('',(0.,0.,1.));
#5137=DIRECTION('center_axis',(1.,0.,0.));
#5138=DIRECTION('ref_axis',(0.,1.,0.));
#5139=DIRECTION('',(0.,1.,0.));
#5140=DIRECTION('',(0.,1.,0.));
#5141=DIRECTION('',(0.,0.,1.));
#5142=DIRECTION('center_axis',(0.,-1.,0.));
#5143=DIRECTION('ref_axis',(1.,0.,0.));
#5144=DIRECTION('',(1.,0.,0.));
#5145=DIRECTION('',(1.,0.,0.));
#5146=DIRECTION('',(0.,0.,1.));
#5147=DIRECTION('center_axis',(-1.,0.,0.));
#5148=DIRECTION('ref_axis',(0.,-1.,0.));
#5149=DIRECTION('',(0.,-1.,0.));
#5150=DIRECTION('',(0.,-1.,0.));
#5151=DIRECTION('center_axis',(0.,0.,1.));
#5152=DIRECTION('ref_axis',(1.,0.,0.));
#5153=DIRECTION('center_axis',(0.,0.,1.));
#5154=DIRECTION('ref_axis',(1.,0.,0.));
#5155=DIRECTION('axis',(0.,0.,1.));
#5156=DIRECTION('refdir',(1.,0.,0.));
#5157=DIRECTION('center_axis',(0.,0.,-1.));
#5158=DIRECTION('ref_axis',(-0.346966786786352,0.93787741675933,0.));
#5159=DIRECTION('',(0.,0.,-1.));
#5160=DIRECTION('center_axis',(0.,0.,-1.));
#5161=DIRECTION('ref_axis',(1.,0.,0.));
#5162=DIRECTION('center_axis',(0.,0.,-1.));
#5163=DIRECTION('ref_axis',(1.,0.,0.));
#5164=DIRECTION('',(0.,0.,-1.));
#5165=DIRECTION('center_axis',(0.,0.,-1.));
#5166=DIRECTION('ref_axis',(1.,0.,0.));
#5167=DIRECTION('',(0.,0.,-1.));
#5168=DIRECTION('center_axis',(0.,0.,-1.));
#5169=DIRECTION('ref_axis',(1.,0.,0.));
#5170=DIRECTION('',(0.,0.,-1.));
#5171=DIRECTION('center_axis',(0.,0.,-1.));
#5172=DIRECTION('ref_axis',(1.,0.,0.));
#5173=DIRECTION('',(0.,0.,-1.));
#5174=DIRECTION('center_axis',(0.,0.,-1.));
#5175=DIRECTION('ref_axis',(1.,0.,0.));
#5176=DIRECTION('',(0.,0.,-1.));
#5177=DIRECTION('center_axis',(0.,0.,-1.));
#5178=DIRECTION('ref_axis',(1.,0.,0.));
#5179=DIRECTION('',(0.,0.,-1.));
#5180=DIRECTION('center_axis',(0.,0.,-1.));
#5181=DIRECTION('ref_axis',(1.,0.,0.));
#5182=DIRECTION('',(0.,0.,-1.));
#5183=DIRECTION('center_axis',(0.,0.,-1.));
#5184=DIRECTION('ref_axis',(1.,0.,0.));
#5185=DIRECTION('',(0.,0.,-1.));
#5186=DIRECTION('center_axis',(0.,0.,-1.));
#5187=DIRECTION('ref_axis',(0.937993686897822,-0.346652337854271,0.));
#5188=DIRECTION('',(0.,0.,-1.));
#5189=DIRECTION('center_axis',(0.,0.,-1.));
#5190=DIRECTION('ref_axis',(1.,0.,0.));
#5191=DIRECTION('center_axis',(0.,0.,-1.));
#5192=DIRECTION('ref_axis',(-0.346967010928538,0.937877333838128,0.));
#5193=DIRECTION('',(0.,0.,-1.));
#5194=DIRECTION('center_axis',(0.,0.,-1.));
#5195=DIRECTION('ref_axis',(1.,0.,0.));
#5196=DIRECTION('center_axis',(0.,0.,-1.));
#5197=DIRECTION('ref_axis',(1.,0.,0.));
#5198=DIRECTION('',(0.,0.,-1.));
#5199=DIRECTION('center_axis',(0.,0.,-1.));
#5200=DIRECTION('ref_axis',(1.,0.,0.));
#5201=DIRECTION('',(0.,0.,-1.));
#5202=DIRECTION('center_axis',(0.,0.,-1.));
#5203=DIRECTION('ref_axis',(1.,0.,0.));
#5204=DIRECTION('',(0.,0.,-1.));
#5205=DIRECTION('center_axis',(0.,0.,-1.));
#5206=DIRECTION('ref_axis',(1.,0.,0.));
#5207=DIRECTION('',(0.,0.,-1.));
#5208=DIRECTION('center_axis',(0.,0.,-1.));
#5209=DIRECTION('ref_axis',(1.,0.,0.));
#5210=DIRECTION('',(0.,0.,-1.));
#5211=DIRECTION('center_axis',(0.,0.,-1.));
#5212=DIRECTION('ref_axis',(1.,0.,0.));
#5213=DIRECTION('',(0.,0.,-1.));
#5214=DIRECTION('center_axis',(0.,0.,-1.));
#5215=DIRECTION('ref_axis',(1.,0.,0.));
#5216=DIRECTION('',(0.,0.,-1.));
#5217=DIRECTION('center_axis',(0.,0.,-1.));
#5218=DIRECTION('ref_axis',(1.,0.,0.));
#5219=DIRECTION('',(0.,0.,-1.));
#5220=DIRECTION('center_axis',(0.,0.,-1.));
#5221=DIRECTION('ref_axis',(0.937993710434555,-0.346652274167091,0.));
#5222=DIRECTION('',(0.,0.,-1.));
#5223=DIRECTION('center_axis',(0.,0.,-1.));
#5224=DIRECTION('ref_axis',(1.,0.,0.));
#5225=DIRECTION('center_axis',(0.,0.,-1.));
#5226=DIRECTION('ref_axis',(-0.346967093288461,0.937877303369133,0.));
#5227=DIRECTION('',(0.,0.,-1.));
#5228=DIRECTION('center_axis',(0.,0.,-1.));
#5229=DIRECTION('ref_axis',(1.,0.,0.));
#5230=DIRECTION('center_axis',(0.,0.,-1.));
#5231=DIRECTION('ref_axis',(1.,0.,0.));
#5232=DIRECTION('',(0.,0.,-1.));
#5233=DIRECTION('center_axis',(0.,0.,-1.));
#5234=DIRECTION('ref_axis',(1.,0.,0.));
#5235=DIRECTION('',(0.,0.,-1.));
#5236=DIRECTION('center_axis',(0.,0.,-1.));
#5237=DIRECTION('ref_axis',(1.,0.,0.));
#5238=DIRECTION('',(0.,0.,-1.));
#5239=DIRECTION('center_axis',(0.,0.,-1.));
#5240=DIRECTION('ref_axis',(1.,0.,0.));
#5241=DIRECTION('',(0.,0.,-1.));
#5242=DIRECTION('center_axis',(0.,0.,-1.));
#5243=DIRECTION('ref_axis',(1.,0.,0.));
#5244=DIRECTION('',(0.,0.,-1.));
#5245=DIRECTION('center_axis',(0.,0.,-1.));
#5246=DIRECTION('ref_axis',(1.,0.,0.));
#5247=DIRECTION('',(0.,0.,-1.));
#5248=DIRECTION('center_axis',(0.,0.,-1.));
#5249=DIRECTION('ref_axis',(1.,0.,0.));
#5250=DIRECTION('',(0.,0.,-1.));
#5251=DIRECTION('center_axis',(0.,0.,-1.));
#5252=DIRECTION('ref_axis',(1.,0.,0.));
#5253=DIRECTION('',(0.,0.,-1.));
#5254=DIRECTION('center_axis',(0.,0.,-1.));
#5255=DIRECTION('ref_axis',(0.937993719003489,-0.346652250980724,0.));
#5256=DIRECTION('',(0.,0.,-1.));
#5257=DIRECTION('center_axis',(0.,0.,-1.));
#5258=DIRECTION('ref_axis',(1.,0.,0.));
#5259=DIRECTION('center_axis',(0.,0.,-1.));
#5260=DIRECTION('ref_axis',(-0.346966676108421,0.93787745770451,0.));
#5261=DIRECTION('',(0.,0.,-1.));
#5262=DIRECTION('center_axis',(0.,0.,-1.));
#5263=DIRECTION('ref_axis',(1.,0.,0.));
#5264=DIRECTION('center_axis',(0.,0.,-1.));
#5265=DIRECTION('ref_axis',(1.,0.,0.));
#5266=DIRECTION('',(0.,0.,-1.));
#5267=DIRECTION('center_axis',(0.,0.,-1.));
#5268=DIRECTION('ref_axis',(1.,0.,0.));
#5269=DIRECTION('',(0.,0.,-1.));
#5270=DIRECTION('center_axis',(0.,0.,-1.));
#5271=DIRECTION('ref_axis',(1.,0.,0.));
#5272=DIRECTION('',(0.,0.,-1.));
#5273=DIRECTION('center_axis',(0.,0.,-1.));
#5274=DIRECTION('ref_axis',(1.,0.,0.));
#5275=DIRECTION('',(0.,0.,-1.));
#5276=DIRECTION('center_axis',(0.,0.,-1.));
#5277=DIRECTION('ref_axis',(1.,0.,0.));
#5278=DIRECTION('',(0.,0.,-1.));
#5279=DIRECTION('center_axis',(0.,0.,-1.));
#5280=DIRECTION('ref_axis',(1.,0.,0.));
#5281=DIRECTION('',(0.,0.,-1.));
#5282=DIRECTION('center_axis',(0.,0.,-1.));
#5283=DIRECTION('ref_axis',(1.,0.,0.));
#5284=DIRECTION('',(0.,0.,-1.));
#5285=DIRECTION('center_axis',(0.,0.,-1.));
#5286=DIRECTION('ref_axis',(1.,0.,0.));
#5287=DIRECTION('',(0.,0.,-1.));
#5288=DIRECTION('center_axis',(0.,0.,-1.));
#5289=DIRECTION('ref_axis',(0.937993675279511,-0.346652369291823,0.));
#5290=DIRECTION('',(0.,0.,-1.));
#5291=DIRECTION('center_axis',(0.,0.,-1.));
#5292=DIRECTION('ref_axis',(1.,0.,0.));
#5293=DIRECTION('center_axis',(0.,0.,-1.));
#5294=DIRECTION('ref_axis',(1.,-4.04571266497536E-14,0.));
#5295=DIRECTION('',(1.22464679914735E-16,-4.9695666632586E-30,-1.));
#5296=DIRECTION('center_axis',(0.,0.,1.));
#5297=DIRECTION('ref_axis',(1.,-4.04571266497536E-14,0.));
#5298=DIRECTION('center_axis',(0.,0.,-1.));
#5299=DIRECTION('ref_axis',(1.,-4.04571266497536E-14,0.));
#5300=DIRECTION('',(1.22464679914735E-16,-4.9695666632586E-30,-1.));
#5301=DIRECTION('center_axis',(0.,0.,-1.));
#5302=DIRECTION('ref_axis',(1.,-4.04571266497536E-14,0.));
#5303=DIRECTION('',(1.22464679914735E-16,-4.9695666632586E-30,-1.));
#5304=DIRECTION('center_axis',(0.,0.,-1.));
#5305=DIRECTION('ref_axis',(1.,-4.04571266497536E-14,0.));
#5306=DIRECTION('',(1.22464679914735E-16,-4.9695666632586E-30,-1.));
#5307=DIRECTION('center_axis',(0.,0.,-1.));
#5308=DIRECTION('ref_axis',(1.,-4.04571266497536E-14,0.));
#5309=DIRECTION('',(1.22464679914735E-16,-4.9695666632586E-30,-1.));
#5310=DIRECTION('center_axis',(0.,0.,-1.));
#5311=DIRECTION('ref_axis',(1.,-4.04571266497536E-14,0.));
#5312=DIRECTION('',(1.22464679914735E-16,-4.9695666632586E-30,-1.));
#5313=DIRECTION('center_axis',(0.,0.,-1.));
#5314=DIRECTION('ref_axis',(1.,-4.04571266497536E-14,0.));
#5315=DIRECTION('',(1.22464679914735E-16,-4.9695666632586E-30,-1.));
#5316=DIRECTION('center_axis',(0.,0.,-1.));
#5317=DIRECTION('ref_axis',(1.,-4.04571266497536E-14,0.));
#5318=DIRECTION('',(1.22464679914735E-16,-4.9695666632586E-30,-1.));
#5319=DIRECTION('center_axis',(0.,0.,-1.));
#5320=DIRECTION('ref_axis',(1.,-4.04571266497536E-14,0.));
#5321=DIRECTION('',(1.22464679914735E-16,-4.9695666632586E-30,-1.));
#5322=DIRECTION('center_axis',(0.,0.,-1.));
#5323=DIRECTION('ref_axis',(-0.609230889865466,-0.792992889522808,0.));
#5324=DIRECTION('',(1.22464679914735E-16,-4.9695666632586E-30,-1.));
#5325=DIRECTION('center_axis',(0.,0.,-1.));
#5326=DIRECTION('ref_axis',(1.,-4.04571266497536E-14,0.));
#5327=DIRECTION('center_axis',(0.,0.,-1.));
#5328=DIRECTION('ref_axis',(1.,-3.75673318890567E-14,0.));
#5329=DIRECTION('',(1.22464679914735E-16,-4.61566887287058E-30,-1.));
#5330=DIRECTION('center_axis',(0.,0.,1.));
#5331=DIRECTION('ref_axis',(1.,-3.75673318890567E-14,0.));
#5332=DIRECTION('center_axis',(0.,0.,-1.));
#5333=DIRECTION('ref_axis',(1.,-3.75673318890567E-14,0.));
#5334=DIRECTION('',(1.22464679914735E-16,-4.61566887287058E-30,-1.));
#5335=DIRECTION('center_axis',(0.,0.,-1.));
#5336=DIRECTION('ref_axis',(1.,-3.75673318890567E-14,0.));
#5337=DIRECTION('',(1.22464679914735E-16,-4.61566887287058E-30,-1.));
#5338=DIRECTION('center_axis',(0.,0.,-1.));
#5339=DIRECTION('ref_axis',(1.,-3.75673318890567E-14,0.));
#5340=DIRECTION('',(1.22464679914735E-16,-4.61566887287058E-30,-1.));
#5341=DIRECTION('center_axis',(0.,0.,-1.));
#5342=DIRECTION('ref_axis',(1.,-3.75673318890567E-14,0.));
#5343=DIRECTION('',(1.22464679914735E-16,-4.61566887287058E-30,-1.));
#5344=DIRECTION('center_axis',(0.,0.,-1.));
#5345=DIRECTION('ref_axis',(1.,-3.75673318890567E-14,0.));
#5346=DIRECTION('',(1.22464679914735E-16,-4.61566887287058E-30,-1.));
#5347=DIRECTION('center_axis',(0.,0.,-1.));
#5348=DIRECTION('ref_axis',(1.,-3.75673318890567E-14,0.));
#5349=DIRECTION('',(1.22464679914735E-16,-4.61566887287058E-30,-1.));
#5350=DIRECTION('center_axis',(0.,0.,-1.));
#5351=DIRECTION('ref_axis',(1.,-3.75673318890567E-14,0.));
#5352=DIRECTION('',(1.22464679914735E-16,-4.61566887287058E-30,-1.));
#5353=DIRECTION('center_axis',(0.,0.,-1.));
#5354=DIRECTION('ref_axis',(1.,-3.75673318890567E-14,0.));
#5355=DIRECTION('',(1.22464679914735E-16,-4.61566887287058E-30,-1.));
#5356=DIRECTION('center_axis',(0.,0.,-1.));
#5357=DIRECTION('ref_axis',(-0.609230947703889,-0.792992845087408,0.));
#5358=DIRECTION('',(1.22464679914735E-16,-4.61566887287058E-30,-1.));
#5359=DIRECTION('center_axis',(0.,0.,-1.));
#5360=DIRECTION('ref_axis',(1.,-3.75673318890567E-14,0.));
#5361=DIRECTION('center_axis',(0.,0.,-1.));
#5362=DIRECTION('ref_axis',(1.,-3.46775371283601E-14,0.));
#5363=DIRECTION('',(1.22464679914735E-16,-4.26177108248259E-30,-1.));
#5364=DIRECTION('center_axis',(0.,0.,1.));
#5365=DIRECTION('ref_axis',(1.,-3.46775371283601E-14,0.));
#5366=DIRECTION('center_axis',(0.,0.,-1.));
#5367=DIRECTION('ref_axis',(1.,-3.46775371283601E-14,0.));
#5368=DIRECTION('',(1.22464679914735E-16,-4.26177108248259E-30,-1.));
#5369=DIRECTION('center_axis',(0.,0.,-1.));
#5370=DIRECTION('ref_axis',(1.,-3.46775371283601E-14,0.));
#5371=DIRECTION('',(1.22464679914735E-16,-4.26177108248259E-30,-1.));
#5372=DIRECTION('center_axis',(0.,0.,-1.));
#5373=DIRECTION('ref_axis',(1.,-3.46775371283601E-14,0.));
#5374=DIRECTION('',(1.22464679914735E-16,-4.26177108248259E-30,-1.));
#5375=DIRECTION('center_axis',(0.,0.,-1.));
#5376=DIRECTION('ref_axis',(1.,-3.46775371283601E-14,0.));
#5377=DIRECTION('',(1.22464679914735E-16,-4.26177108248259E-30,-1.));
#5378=DIRECTION('center_axis',(0.,0.,-1.));
#5379=DIRECTION('ref_axis',(1.,-3.46775371283601E-14,0.));
#5380=DIRECTION('',(1.22464679914735E-16,-4.26177108248259E-30,-1.));
#5381=DIRECTION('center_axis',(0.,0.,-1.));
#5382=DIRECTION('ref_axis',(1.,-3.46775371283601E-14,0.));
#5383=DIRECTION('',(1.22464679914735E-16,-4.26177108248259E-30,-1.));
#5384=DIRECTION('center_axis',(0.,0.,-1.));
#5385=DIRECTION('ref_axis',(1.,-3.46775371283601E-14,0.));
#5386=DIRECTION('',(1.22464679914735E-16,-4.26177108248259E-30,-1.));
#5387=DIRECTION('center_axis',(0.,0.,-1.));
#5388=DIRECTION('ref_axis',(1.,-3.46775371283601E-14,0.));
#5389=DIRECTION('',(1.22464679914735E-16,-4.26177108248259E-30,-1.));
#5390=DIRECTION('center_axis',(0.,0.,-1.));
#5391=DIRECTION('ref_axis',(-0.609230907205664,-0.792992876200892,0.));
#5392=DIRECTION('',(1.22464679914735E-16,-4.26177108248259E-30,-1.));
#5393=DIRECTION('center_axis',(0.,0.,-1.));
#5394=DIRECTION('ref_axis',(1.,-3.46775371283601E-14,0.));
#5395=DIRECTION('center_axis',(0.,0.,-1.));
#5396=DIRECTION('ref_axis',(1.,-3.17877423676634E-14,0.));
#5397=DIRECTION('',(1.22464679914735E-16,-3.90787329209458E-30,-1.));
#5398=DIRECTION('center_axis',(0.,0.,1.));
#5399=DIRECTION('ref_axis',(1.,-3.17877423676634E-14,0.));
#5400=DIRECTION('center_axis',(0.,0.,-1.));
#5401=DIRECTION('ref_axis',(1.,-3.17877423676634E-14,0.));
#5402=DIRECTION('',(1.22464679914735E-16,-3.90787329209458E-30,-1.));
#5403=DIRECTION('center_axis',(0.,0.,-1.));
#5404=DIRECTION('ref_axis',(1.,-3.17877423676634E-14,0.));
#5405=DIRECTION('',(1.22464679914735E-16,-3.90787329209458E-30,-1.));
#5406=DIRECTION('center_axis',(0.,0.,-1.));
#5407=DIRECTION('ref_axis',(1.,-3.17877423676634E-14,0.));
#5408=DIRECTION('',(1.22464679914735E-16,-3.90787329209458E-30,-1.));
#5409=DIRECTION('center_axis',(0.,0.,-1.));
#5410=DIRECTION('ref_axis',(1.,-3.17877423676634E-14,0.));
#5411=DIRECTION('',(1.22464679914735E-16,-3.90787329209458E-30,-1.));
#5412=DIRECTION('center_axis',(0.,0.,-1.));
#5413=DIRECTION('ref_axis',(1.,-3.17877423676634E-14,0.));
#5414=DIRECTION('',(1.22464679914735E-16,-3.90787329209458E-30,-1.));
#5415=DIRECTION('center_axis',(0.,0.,-1.));
#5416=DIRECTION('ref_axis',(1.,-3.17877423676634E-14,0.));
#5417=DIRECTION('',(1.22464679914735E-16,-3.90787329209458E-30,-1.));
#5418=DIRECTION('center_axis',(0.,0.,-1.));
#5419=DIRECTION('ref_axis',(1.,-3.17877423676634E-14,0.));
#5420=DIRECTION('',(1.22464679914735E-16,-3.90787329209458E-30,-1.));
#5421=DIRECTION('center_axis',(0.,0.,-1.));
#5422=DIRECTION('ref_axis',(1.,-3.17877423676634E-14,0.));
#5423=DIRECTION('',(1.22464679914735E-16,-3.90787329209458E-30,-1.));
#5424=DIRECTION('center_axis',(0.,0.,-1.));
#5425=DIRECTION('ref_axis',(-0.609230926478059,-0.792992861394531,0.));
#5426=DIRECTION('',(1.22464679914735E-16,-3.90787329209458E-30,-1.));
#5427=DIRECTION('center_axis',(0.,0.,-1.));
#5428=DIRECTION('ref_axis',(1.,-3.17877423676634E-14,0.));
#5429=DIRECTION('center_axis',(0.,0.,-1.));
#5430=DIRECTION('ref_axis',(1.,-3.17877423676634E-14,0.));
#5431=DIRECTION('center_axis',(0.,0.,1.));
#5432=DIRECTION('ref_axis',(1.,0.,0.));
#5433=DIRECTION('',(0.,-1.,0.));
#5434=DIRECTION('',(1.,0.,0.));
#5435=DIRECTION('',(0.,1.,0.));
#5436=DIRECTION('',(-1.,0.,0.));
#5437=DIRECTION('center_axis',(0.,0.,-1.));
#5438=DIRECTION('ref_axis',(1.,-3.46775371283601E-14,0.));
#5439=DIRECTION('center_axis',(0.,0.,-1.));
#5440=DIRECTION('ref_axis',(1.,-3.75673318890567E-14,0.));
#5441=DIRECTION('center_axis',(0.,0.,-1.));
#5442=DIRECTION('ref_axis',(1.,-4.04571266497536E-14,0.));
#5443=DIRECTION('center_axis',(0.,0.,-1.));
#5444=DIRECTION('ref_axis',(1.,0.,0.));
#5445=DIRECTION('center_axis',(0.,0.,-1.));
#5446=DIRECTION('ref_axis',(1.,0.,0.));
#5447=DIRECTION('center_axis',(0.,0.,-1.));
#5448=DIRECTION('ref_axis',(1.,0.,0.));
#5449=DIRECTION('center_axis',(0.,0.,-1.));
#5450=DIRECTION('ref_axis',(1.,0.,0.));
#5451=DIRECTION('center_axis',(0.,1.,0.));
#5452=DIRECTION('ref_axis',(-1.,0.,0.));
#5453=DIRECTION('',(-1.,0.,0.));
#5454=DIRECTION('',(0.,0.,1.));
#5455=DIRECTION('',(0.,0.,1.));
#5456=DIRECTION('center_axis',(1.,0.,0.));
#5457=DIRECTION('ref_axis',(0.,1.,0.));
#5458=DIRECTION('',(0.,1.,0.));
#5459=DIRECTION('',(0.,0.,1.));
#5460=DIRECTION('center_axis',(0.,-1.,0.));
#5461=DIRECTION('ref_axis',(1.,0.,0.));
#5462=DIRECTION('',(1.,0.,0.));
#5463=DIRECTION('',(0.,0.,1.));
#5464=DIRECTION('center_axis',(-1.,0.,0.));
#5465=DIRECTION('ref_axis',(0.,-1.,0.));
#5466=DIRECTION('',(0.,-1.,0.));
#5467=DIRECTION('center_axis',(0.,0.,1.));
#5468=DIRECTION('ref_axis',(1.,0.,0.));
#5469=DIRECTION('axis',(0.,0.,1.));
#5470=DIRECTION('refdir',(1.,0.,0.));
#5471=DIRECTION('center_axis',(0.,1.,0.));
#5472=DIRECTION('ref_axis',(-1.,0.,0.));
#5473=DIRECTION('',(-1.,0.,0.));
#5474=DIRECTION('',(0.,0.,1.));
#5475=DIRECTION('',(-1.,0.,0.));
#5476=DIRECTION('',(0.,0.,1.));
#5477=DIRECTION('center_axis',(1.,0.,0.));
#5478=DIRECTION('ref_axis',(0.,1.,0.));
#5479=DIRECTION('',(0.,1.,0.));
#5480=DIRECTION('',(0.,1.,0.));
#5481=DIRECTION('',(0.,0.,1.));
#5482=DIRECTION('center_axis',(0.,-1.,0.));
#5483=DIRECTION('ref_axis',(1.,0.,0.));
#5484=DIRECTION('',(1.,0.,0.));
#5485=DIRECTION('',(1.,0.,0.));
#5486=DIRECTION('',(0.,0.,1.));
#5487=DIRECTION('center_axis',(-1.,0.,0.));
#5488=DIRECTION('ref_axis',(0.,-1.,0.));
#5489=DIRECTION('',(0.,-1.,0.));
#5490=DIRECTION('',(0.,-1.,0.));
#5491=DIRECTION('center_axis',(0.,0.,1.));
#5492=DIRECTION('ref_axis',(1.,0.,0.));
#5493=DIRECTION('center_axis',(0.,0.,1.));
#5494=DIRECTION('ref_axis',(1.,0.,0.));
#5495=DIRECTION('axis',(0.,0.,1.));
#5496=DIRECTION('refdir',(1.,0.,0.));
#5497=DIRECTION('center_axis',(0.,0.,1.));
#5498=DIRECTION('ref_axis',(1.,0.,0.));
#5499=DIRECTION('center_axis',(0.,0.,-1.));
#5500=DIRECTION('ref_axis',(1.,0.,0.));
#5501=DIRECTION('',(0.,0.,-1.));
#5502=DIRECTION('center_axis',(0.,0.,-1.));
#5503=DIRECTION('ref_axis',(1.,0.,0.));
#5504=DIRECTION('center_axis',(0.,0.,1.));
#5505=DIRECTION('ref_axis',(1.,0.,0.));
#5506=DIRECTION('center_axis',(0.,0.,1.));
#5507=DIRECTION('ref_axis',(1.,0.,0.));
#5508=DIRECTION('',(0.,0.,-1.));
#5509=DIRECTION('center_axis',(0.,0.,1.));
#5510=DIRECTION('ref_axis',(1.,0.,0.));
#5511=DIRECTION('center_axis',(0.,0.,1.));
#5512=DIRECTION('ref_axis',(1.,0.,0.));
#5513=DIRECTION('center_axis',(0.,0.,1.));
#5514=DIRECTION('ref_axis',(1.,0.,0.));
#5515=DIRECTION('axis',(0.,0.,1.));
#5516=DIRECTION('refdir',(1.,0.,0.));
#5517=DIRECTION('center_axis',(0.,0.,1.));
#5518=DIRECTION('ref_axis',(1.,0.,0.));
#5519=DIRECTION('center_axis',(0.,0.,-1.));
#5520=DIRECTION('ref_axis',(1.,0.,0.));
#5521=DIRECTION('',(0.,0.,-1.));
#5522=DIRECTION('center_axis',(0.,0.,-1.));
#5523=DIRECTION('ref_axis',(1.,0.,0.));
#5524=DIRECTION('center_axis',(0.,0.,1.));
#5525=DIRECTION('ref_axis',(1.,0.,0.));
#5526=DIRECTION('center_axis',(0.,0.,1.));
#5527=DIRECTION('ref_axis',(1.,0.,0.));
#5528=DIRECTION('',(0.,0.,-1.));
#5529=DIRECTION('center_axis',(0.,0.,1.));
#5530=DIRECTION('ref_axis',(1.,0.,0.));
#5531=DIRECTION('center_axis',(0.,0.,1.));
#5532=DIRECTION('ref_axis',(1.,0.,0.));
#5533=DIRECTION('center_axis',(0.,0.,1.));
#5534=DIRECTION('ref_axis',(1.,0.,0.));
#5535=DIRECTION('axis',(0.,0.,1.));
#5536=DIRECTION('refdir',(1.,0.,0.));
#5537=DIRECTION('center_axis',(0.,0.,1.));
#5538=DIRECTION('ref_axis',(1.,0.,0.));
#5539=DIRECTION('center_axis',(0.,0.,1.));
#5540=DIRECTION('ref_axis',(1.,0.,0.));
#5541=DIRECTION('',(0.,0.,1.));
#5542=DIRECTION('center_axis',(0.,0.,1.));
#5543=DIRECTION('ref_axis',(1.,0.,0.));
#5544=DIRECTION('center_axis',(0.,0.,-1.));
#5545=DIRECTION('ref_axis',(-1.,0.,0.));
#5546=DIRECTION('center_axis',(0.,0.,-1.));
#5547=DIRECTION('ref_axis',(1.,0.,0.));
#5548=DIRECTION('center_axis',(0.,0.,1.));
#5549=DIRECTION('ref_axis',(1.,0.,0.));
#5550=DIRECTION('center_axis',(0.,0.,1.));
#5551=DIRECTION('ref_axis',(1.,0.,0.));
#5552=DIRECTION('center_axis',(0.,0.,1.));
#5553=DIRECTION('ref_axis',(1.,0.,0.));
#5554=DIRECTION('center_axis',(0.,0.,1.));
#5555=DIRECTION('ref_axis',(1.,0.,0.));
#5556=DIRECTION('',(0.,0.,-1.));
#5557=DIRECTION('center_axis',(0.,0.,1.));
#5558=DIRECTION('ref_axis',(1.,0.,0.));
#5559=DIRECTION('center_axis',(0.,0.,1.));
#5560=DIRECTION('ref_axis',(1.,0.,0.));
#5561=DIRECTION('center_axis',(0.,0.,1.));
#5562=DIRECTION('ref_axis',(1.,0.,0.));
#5563=DIRECTION('center_axis',(0.,0.,1.));
#5564=DIRECTION('ref_axis',(1.,0.,0.));
#5565=DIRECTION('',(0.,0.,-1.));
#5566=DIRECTION('center_axis',(0.,0.,1.));
#5567=DIRECTION('ref_axis',(1.,0.,0.));
#5568=DIRECTION('center_axis',(0.,0.,1.));
#5569=DIRECTION('ref_axis',(1.,0.,0.));
#5570=DIRECTION('center_axis',(0.,0.,1.));
#5571=DIRECTION('ref_axis',(1.,0.,0.));
#5572=DIRECTION('',(0.,0.,-1.));
#5573=DIRECTION('center_axis',(0.,0.,1.));
#5574=DIRECTION('ref_axis',(1.,0.,0.));
#5575=DIRECTION('axis',(0.,0.,1.));
#5576=DIRECTION('refdir',(1.,0.,0.));
#5577=DIRECTION('center_axis',(-1.,0.,0.));
#5578=DIRECTION('ref_axis',(0.,1.,0.));
#5579=DIRECTION('',(0.,0.,1.));
#5580=DIRECTION('',(0.,-1.,0.));
#5581=DIRECTION('',(0.,0.,-1.));
#5582=DIRECTION('',(0.,1.,0.));
#5583=DIRECTION('center_axis',(1.,0.,0.));
#5584=DIRECTION('ref_axis',(0.,-1.,0.));
#5585=DIRECTION('',(0.,0.,-1.));
#5586=DIRECTION('',(0.,-1.,0.));
#5587=DIRECTION('',(0.,0.,1.));
#5588=DIRECTION('',(0.,1.,0.));
#5589=DIRECTION('center_axis',(0.,0.,1.));
#5590=DIRECTION('ref_axis',(1.,0.,0.));
#5591=DIRECTION('center_axis',(0.,0.,1.));
#5592=DIRECTION('ref_axis',(1.,0.,0.));
#5593=DIRECTION('center_axis',(0.,0.,-1.));
#5594=DIRECTION('ref_axis',(1.,0.,0.));
#5595=DIRECTION('center_axis',(0.,0.,1.));
#5596=DIRECTION('ref_axis',(6.12323399573677E-17,-1.,0.));
#5597=DIRECTION('center_axis',(0.,0.,-1.));
#5598=DIRECTION('ref_axis',(1.,0.,0.));
#5599=DIRECTION('center_axis',(0.,0.,1.));
#5600=DIRECTION('ref_axis',(6.12323399573677E-17,-1.,0.));
#5601=DIRECTION('center_axis',(0.,0.,1.));
#5602=DIRECTION('ref_axis',(1.,0.,0.));
#5603=DIRECTION('center_axis',(0.,0.,1.));
#5604=DIRECTION('ref_axis',(1.,0.,0.));
#5605=DIRECTION('axis',(0.,0.,1.));
#5606=DIRECTION('refdir',(1.,0.,0.));
#5607=DIRECTION('center_axis',(0.,0.,1.));
#5608=DIRECTION('ref_axis',(1.,0.,0.));
#5609=DIRECTION('center_axis',(0.,0.,-1.));
#5610=DIRECTION('ref_axis',(1.,0.,0.));
#5611=DIRECTION('',(0.,0.,-1.));
#5612=DIRECTION('center_axis',(0.,0.,-1.));
#5613=DIRECTION('ref_axis',(1.,0.,0.));
#5614=DIRECTION('center_axis',(0.,0.,1.));
#5615=DIRECTION('ref_axis',(1.,0.,0.));
#5616=DIRECTION('center_axis',(0.,0.,1.));
#5617=DIRECTION('ref_axis',(1.,0.,0.));
#5618=DIRECTION('',(0.,0.,-1.));
#5619=DIRECTION('center_axis',(0.,0.,1.));
#5620=DIRECTION('ref_axis',(1.,0.,0.));
#5621=DIRECTION('center_axis',(0.,0.,1.));
#5622=DIRECTION('ref_axis',(1.,0.,0.));
#5623=DIRECTION('center_axis',(0.,0.,1.));
#5624=DIRECTION('ref_axis',(1.,0.,0.));
#5625=DIRECTION('axis',(0.,0.,1.));
#5626=DIRECTION('refdir',(1.,0.,0.));
#5627=DIRECTION('center_axis',(0.,0.,1.));
#5628=DIRECTION('ref_axis',(1.,0.,0.));
#5629=DIRECTION('center_axis',(0.,0.,-1.));
#5630=DIRECTION('ref_axis',(1.,0.,0.));
#5631=DIRECTION('',(0.,0.,-1.));
#5632=DIRECTION('center_axis',(0.,0.,-1.));
#5633=DIRECTION('ref_axis',(1.,0.,0.));
#5634=DIRECTION('center_axis',(0.,0.,1.));
#5635=DIRECTION('ref_axis',(1.,0.,0.));
#5636=DIRECTION('center_axis',(0.,0.,1.));
#5637=DIRECTION('ref_axis',(1.,0.,0.));
#5638=DIRECTION('',(0.,0.,-1.));
#5639=DIRECTION('center_axis',(0.,0.,1.));
#5640=DIRECTION('ref_axis',(1.,0.,0.));
#5641=DIRECTION('center_axis',(0.,0.,1.));
#5642=DIRECTION('ref_axis',(1.,0.,0.));
#5643=DIRECTION('center_axis',(0.,0.,1.));
#5644=DIRECTION('ref_axis',(1.,0.,0.));
#5645=DIRECTION('axis',(0.,0.,1.));
#5646=DIRECTION('refdir',(1.,0.,0.));
#5647=DIRECTION('center_axis',(0.,0.,1.));
#5648=DIRECTION('ref_axis',(1.,0.,0.));
#5649=DIRECTION('center_axis',(0.,0.,-1.));
#5650=DIRECTION('ref_axis',(1.,0.,0.));
#5651=DIRECTION('',(0.,0.,-1.));
#5652=DIRECTION('center_axis',(0.,0.,-1.));
#5653=DIRECTION('ref_axis',(1.,0.,0.));
#5654=DIRECTION('center_axis',(0.,0.,1.));
#5655=DIRECTION('ref_axis',(1.,0.,0.));
#5656=DIRECTION('center_axis',(0.,0.,1.));
#5657=DIRECTION('ref_axis',(1.,0.,0.));
#5658=DIRECTION('',(0.,0.,-1.));
#5659=DIRECTION('center_axis',(0.,0.,1.));
#5660=DIRECTION('ref_axis',(1.,0.,0.));
#5661=DIRECTION('center_axis',(0.,0.,1.));
#5662=DIRECTION('ref_axis',(1.,0.,0.));
#5663=DIRECTION('center_axis',(0.,0.,1.));
#5664=DIRECTION('ref_axis',(1.,0.,0.));
#5665=DIRECTION('',(0.,0.,1.));
#5666=DIRECTION('',(1.,0.,0.));
#5667=DIRECTION('',(1.,0.,0.));
#5668=DIRECTION('',(0.,1.,0.));
#5669=DIRECTION('',(0.,0.,1.));
#5670=DIRECTION('',(1.,0.,0.));
#5671=DIRECTION('',(0.,0.,1.));
#5672=DIRECTION('',(1.,0.,0.));
#5673=DIRECTION('',(0.,0.,1.));
#5674=DIRECTION('',(1.,0.,0.));
#5675=DIRECTION('',(1.,0.,0.));
#5676=DIRECTION('',(0.,1.,0.));
#5677=DIRECTION('',(0.,0.,1.));
#5678=DIRECTION('',(1.,0.,0.));
#5679=DIRECTION('',(6.12323399573677E-17,-6.12323399573677E-17,1.));
#5680=DIRECTION('',(1.,6.12323399573677E-17,-6.12323399573677E-17));
#5681=DIRECTION('',(6.12323399573677E-17,-6.12323399573677E-17,1.));
#5682=DIRECTION('',(1.,6.12323399573677E-17,-6.12323399573677E-17));
#5683=DIRECTION('',(6.12323399573677E-17,-6.12323399573677E-17,1.));
#5684=DIRECTION('',(1.,6.12323399573677E-17,-6.12323399573677E-17));
#5685=DIRECTION('',(-1.51183490939638E-16,1.,-2.20179555167574E-16));
#5686=DIRECTION('',(-0.991600562145614,-1.21436045416245E-16,0.129338026707168));
#5687=DIRECTION('',(-1.51183490939638E-16,1.,-2.20179555167574E-16));
#5688=DIRECTION('',(-0.991600562145614,-1.21436045416245E-16,0.129338026707168));
#5689=DIRECTION('',(-6.12323399573676E-17,1.,2.83276944882399E-16));
#5690=DIRECTION('',(1.,6.12323399573677E-17,-6.12323399573677E-17));
#5691=DIRECTION('',(-6.12323399573676E-17,1.,2.83276944882399E-16));
#5692=DIRECTION('',(1.,6.12323399573677E-17,-6.12323399573677E-17));
#5693=DIRECTION('',(-6.12323399573676E-17,1.,2.83276944882399E-16));
#5694=DIRECTION('',(1.,6.12323399573677E-17,-6.12323399573677E-17));
#5695=DIRECTION('',(-6.12323399573676E-17,1.,2.83276944882399E-16));
#5696=DIRECTION('',(1.,6.12323399573677E-17,-6.12323399573677E-17));
#5697=DIRECTION('',(-6.12323399573676E-17,1.,2.83276944882399E-16));
#5698=DIRECTION('',(1.,6.12323399573677E-17,-6.12323399573677E-17));
#5699=DIRECTION('',(0.,0.,1.));
#5700=DIRECTION('',(1.,0.,0.));
#5701=DIRECTION('',(0.,0.,1.));
#5702=DIRECTION('',(1.,0.,0.));
#5703=DIRECTION('',(1.,0.,0.));
#5704=DIRECTION('',(0.,1.,0.));
#5705=DIRECTION('',(0.,0.,1.));
#5706=DIRECTION('',(1.,0.,0.));
#5707=DIRECTION('',(6.12323399573677E-17,-6.12323399573677E-17,1.));
#5708=DIRECTION('',(1.,6.12323399573677E-17,-6.12323399573677E-17));
#5709=DIRECTION('',(6.12323399573677E-17,-6.12323399573677E-17,1.));
#5710=DIRECTION('',(1.,6.12323399573677E-17,-6.12323399573677E-17));
#5711=DIRECTION('',(6.12323399573677E-17,-6.12323399573677E-17,1.));
#5712=DIRECTION('',(1.,6.12323399573677E-17,-6.12323399573677E-17));
#5713=DIRECTION('',(-6.12323399573676E-17,1.,2.83276944882399E-16));
#5714=DIRECTION('',(1.,6.12323399573677E-17,-6.12323399573677E-17));
#5715=DIRECTION('',(-6.12323399573676E-17,1.,2.83276944882399E-16));
#5716=DIRECTION('',(1.,6.12323399573677E-17,-6.12323399573677E-17));
#5717=DIRECTION('',(-6.12323399573676E-17,1.,2.83276944882399E-16));
#5718=DIRECTION('',(1.,6.12323399573677E-17,-6.12323399573677E-17));
#5719=DIRECTION('',(-1.51183490939638E-16,1.,-2.20179555167574E-16));
#5720=DIRECTION('',(-0.991600562145614,-1.21436045416245E-16,0.129338026707168));
#5721=DIRECTION('',(-1.51183490939638E-16,1.,-2.20179555167574E-16));
#5722=DIRECTION('',(-0.991600562145614,-1.21436045416245E-16,0.129338026707168));
#5723=DIRECTION('',(-6.12323399573676E-17,1.,2.83276944882399E-16));
#5724=DIRECTION('',(1.,6.12323399573677E-17,-6.12323399573677E-17));
#5725=DIRECTION('',(-6.12323399573676E-17,1.,2.83276944882399E-16));
#5726=DIRECTION('',(1.,6.12323399573677E-17,-6.12323399573677E-17));
#5727=DIRECTION('',(-6.12323399573676E-17,1.,2.83276944882399E-16));
#5728=DIRECTION('',(1.,6.12323399573677E-17,-6.12323399573677E-17));
#5729=DIRECTION('',(-6.12323399573676E-17,1.,2.83276944882399E-16));
#5730=DIRECTION('',(1.,6.12323399573677E-17,-6.12323399573677E-17));
#5731=DIRECTION('',(-6.12323399573676E-17,1.,2.83276944882399E-16));
#5732=DIRECTION('',(1.,6.12323399573677E-17,-6.12323399573677E-17));
#5733=DIRECTION('',(-6.12323399573676E-17,1.,2.83276944882399E-16));
#5734=DIRECTION('',(1.,6.12323399573677E-17,-6.12323399573677E-17));
#5735=DIRECTION('',(-6.12323399573676E-17,1.,2.83276944882399E-16));
#5736=DIRECTION('',(1.,6.12323399573677E-17,-6.12323399573677E-17));
#5737=DIRECTION('',(-6.12323399573676E-17,1.,2.83276944882399E-16));
#5738=DIRECTION('',(1.,6.12323399573677E-17,-6.12323399573677E-17));
#5739=DIRECTION('',(-9.3745868855685E-17,1.,-2.2017955496255E-16));
#5740=DIRECTION('',(-0.991600562145614,-1.21436045416245E-16,-0.129338026707169));
#5741=DIRECTION('',(-9.3745868855685E-17,1.,-2.2017955496255E-16));
#5742=DIRECTION('',(-0.991600562145614,-1.21436045416245E-16,-0.129338026707169));
#5743=DIRECTION('',(-6.12323399573676E-17,1.,2.83276944882399E-16));
#5744=DIRECTION('',(1.,6.12323399573677E-17,-6.12323399573677E-17));
#5745=DIRECTION('',(-6.12323399573676E-17,1.,2.83276944882399E-16));
#5746=DIRECTION('',(1.,6.12323399573677E-17,-6.12323399573677E-17));
#5747=DIRECTION('',(-6.12323399573676E-17,1.,2.83276944882399E-16));
#5748=DIRECTION('',(1.,6.12323399573677E-17,-6.12323399573677E-17));
#5749=DIRECTION('',(-6.12323399573676E-17,1.,2.83276944882399E-16));
#5750=DIRECTION('',(1.,6.12323399573677E-17,-6.12323399573677E-17));
#5751=DIRECTION('',(-6.12323399573676E-17,1.,2.83276944882399E-16));
#5752=DIRECTION('',(1.,6.12323399573677E-17,-6.12323399573677E-17));
#5753=DIRECTION('',(-6.12323399573676E-17,1.,2.83276944882399E-16));
#5754=DIRECTION('',(1.,6.12323399573677E-17,-6.12323399573677E-17));
#5755=DIRECTION('',(-6.12323399573676E-17,1.,2.83276944882399E-16));
#5756=DIRECTION('',(1.,6.12323399573677E-17,-6.12323399573677E-17));
#5757=DIRECTION('',(-6.12323399573676E-17,1.,2.83276944882399E-16));
#5758=DIRECTION('',(1.,6.12323399573677E-17,-6.12323399573677E-17));
#5759=DIRECTION('',(-9.3745868855685E-17,1.,-2.2017955496255E-16));
#5760=DIRECTION('',(-0.991600562145614,-1.21436045416245E-16,-0.129338026707169));
#5761=DIRECTION('',(-9.3745868855685E-17,1.,-2.2017955496255E-16));
#5762=DIRECTION('',(-0.991600562145614,-1.21436045416245E-16,-0.129338026707169));
#5763=DIRECTION('',(-6.12323399573676E-17,1.,2.83276944882399E-16));
#5764=DIRECTION('',(1.,6.12323399573677E-17,-6.12323399573677E-17));
#5765=DIRECTION('',(-6.12323399573676E-17,1.,2.83276944882399E-16));
#5766=DIRECTION('',(1.,6.12323399573677E-17,-6.12323399573677E-17));
#5767=DIRECTION('',(-6.12323399573676E-17,1.,2.83276944882399E-16));
#5768=DIRECTION('',(1.,6.12323399573677E-17,-6.12323399573677E-17));
#5769=DIRECTION('',(-6.12323399573676E-17,1.,2.83276944882399E-16));
#5770=DIRECTION('',(1.,6.12323399573677E-17,-6.12323399573677E-17));
#5771=DIRECTION('',(-6.12323399573676E-17,1.,2.83276944882399E-16));
#5772=DIRECTION('',(1.,6.12323399573677E-17,-6.12323399573677E-17));
#5773=DIRECTION('',(-6.12323399573676E-17,1.,2.83276944882399E-16));
#5774=DIRECTION('',(1.,6.12323399573677E-17,-6.12323399573677E-17));
#5775=DIRECTION('',(-6.12323399573676E-17,1.,2.83276944882399E-16));
#5776=DIRECTION('',(1.,6.12323399573677E-17,-6.12323399573677E-17));
#5777=DIRECTION('',(-6.12323399573676E-17,1.,2.83276944882399E-16));
#5778=DIRECTION('',(1.,6.12323399573677E-17,-6.12323399573677E-17));
#5779=CARTESIAN_POINT('',(0.,0.,0.));
#5780=CARTESIAN_POINT('',(0.,0.,0.));
#5781=CARTESIAN_POINT('Origin',(-39.,-19.,0.));
#5782=CARTESIAN_POINT('',(-39.,-20.,400.));
#5783=CARTESIAN_POINT('',(-40.,-19.,400.));
#5784=CARTESIAN_POINT('Origin',(-39.,-19.,400.));
#5785=CARTESIAN_POINT('',(-40.,-19.,0.));
#5786=CARTESIAN_POINT('',(-40.,-19.,0.));
#5787=CARTESIAN_POINT('',(-39.,-20.,0.));
#5788=CARTESIAN_POINT('Origin',(-39.,-19.,0.));
#5789=CARTESIAN_POINT('',(-39.,-20.,0.));
#5790=CARTESIAN_POINT('Origin',(-40.,20.,0.));
#5791=CARTESIAN_POINT('',(-40.,19.,400.));
#5792=CARTESIAN_POINT('',(-40.,20.,400.));
#5793=CARTESIAN_POINT('',(-40.,19.,0.));
#5794=CARTESIAN_POINT('',(-40.,19.,0.));
#5795=CARTESIAN_POINT('',(-40.,20.,0.));
#5796=CARTESIAN_POINT('Origin',(0.,0.,400.));
#5797=CARTESIAN_POINT('',(39.,-20.,400.));
#5798=CARTESIAN_POINT('',(-40.,-20.,400.));
#5799=CARTESIAN_POINT('',(40.,-19.,400.));
#5800=CARTESIAN_POINT('Origin',(39.,-19.,400.));
#5801=CARTESIAN_POINT('',(40.,19.,400.));
#5802=CARTESIAN_POINT('',(40.,-20.,400.));
#5803=CARTESIAN_POINT('',(39.,20.,400.));
#5804=CARTESIAN_POINT('Origin',(39.,19.,400.));
#5805=CARTESIAN_POINT('',(-39.,20.,400.));
#5806=CARTESIAN_POINT('',(40.,20.,400.));
#5807=CARTESIAN_POINT('Origin',(-39.,19.,400.));
#5808=CARTESIAN_POINT('',(-36.,-15.,400.));
#5809=CARTESIAN_POINT('',(-36.,15.,400.));
#5810=CARTESIAN_POINT('',(-36.,16.,400.));
#5811=CARTESIAN_POINT('',(-35.,16.,400.));
#5812=CARTESIAN_POINT('Origin',(-35.,15.,400.));
#5813=CARTESIAN_POINT('',(35.,16.,400.));
#5814=CARTESIAN_POINT('',(36.,16.,400.));
#5815=CARTESIAN_POINT('',(36.,15.,400.));
#5816=CARTESIAN_POINT('Origin',(35.,15.,400.));
#5817=CARTESIAN_POINT('',(36.,-15.,400.));
#5818=CARTESIAN_POINT('',(36.,-16.,400.));
#5819=CARTESIAN_POINT('',(35.,-16.,400.));
#5820=CARTESIAN_POINT('Origin',(35.,-15.,400.));
#5821=CARTESIAN_POINT('',(-35.,-16.,400.));
#5822=CARTESIAN_POINT('',(-36.,-16.,400.));
#5823=CARTESIAN_POINT('Origin',(-35.,-15.,400.));
#5824=CARTESIAN_POINT('Origin',(39.,-19.,0.));
#5825=CARTESIAN_POINT('',(39.,-20.,0.));
#5826=CARTESIAN_POINT('',(39.,-20.,0.));
#5827=CARTESIAN_POINT('',(40.,-19.,0.));
#5828=CARTESIAN_POINT('Origin',(39.,-19.,0.));
#5829=CARTESIAN_POINT('',(40.,-19.,0.));
#5830=CARTESIAN_POINT('Origin',(40.,-20.,0.));
#5831=CARTESIAN_POINT('',(40.,19.,0.));
#5832=CARTESIAN_POINT('',(40.,-20.,0.));
#5833=CARTESIAN_POINT('',(40.,19.,0.));
#5834=CARTESIAN_POINT('Origin',(39.,19.,0.));
#5835=CARTESIAN_POINT('',(39.,20.,0.));
#5836=CARTESIAN_POINT('Origin',(39.,19.,0.));
#5837=CARTESIAN_POINT('',(39.,20.,0.));
#5838=CARTESIAN_POINT('Origin',(-39.,19.,0.));
#5839=CARTESIAN_POINT('',(-39.,20.,0.));
#5840=CARTESIAN_POINT('',(-39.,20.,0.));
#5841=CARTESIAN_POINT('Origin',(-39.,19.,0.));
#5842=CARTESIAN_POINT('Origin',(-35.,15.,0.));
#5843=CARTESIAN_POINT('',(-36.,15.,0.));
#5844=CARTESIAN_POINT('',(-35.,16.,0.));
#5845=CARTESIAN_POINT('Origin',(-35.,15.,0.));
#5846=CARTESIAN_POINT('',(-35.,16.,0.));
#5847=CARTESIAN_POINT('',(-36.,15.,0.));
#5848=CARTESIAN_POINT('Origin',(-36.,16.,0.));
#5849=CARTESIAN_POINT('',(35.,16.,0.));
#5850=CARTESIAN_POINT('',(36.,16.,0.));
#5851=CARTESIAN_POINT('',(35.,16.,0.));
#5852=CARTESIAN_POINT('Origin',(35.,15.,0.));
#5853=CARTESIAN_POINT('',(36.,15.,0.));
#5854=CARTESIAN_POINT('Origin',(35.,15.,0.));
#5855=CARTESIAN_POINT('',(36.,15.,0.));
#5856=CARTESIAN_POINT('Origin',(36.,16.,0.));
#5857=CARTESIAN_POINT('',(36.,-15.,0.));
#5858=CARTESIAN_POINT('',(36.,-16.,0.));
#5859=CARTESIAN_POINT('',(36.,-15.,0.));
#5860=CARTESIAN_POINT('Origin',(35.,-15.,0.));
#5861=CARTESIAN_POINT('',(35.,-16.,0.));
#5862=CARTESIAN_POINT('Origin',(35.,-15.,0.));
#5863=CARTESIAN_POINT('',(35.,-16.,0.));
#5864=CARTESIAN_POINT('Origin',(36.,-16.,0.));
#5865=CARTESIAN_POINT('',(-35.,-16.,0.));
#5866=CARTESIAN_POINT('',(-36.,-16.,0.));
#5867=CARTESIAN_POINT('',(-35.,-16.,0.));
#5868=CARTESIAN_POINT('Origin',(-35.,-15.,0.));
#5869=CARTESIAN_POINT('',(-36.,-15.,0.));
#5870=CARTESIAN_POINT('Origin',(-35.,-15.,0.));
#5871=CARTESIAN_POINT('',(-36.,-15.,0.));
#5872=CARTESIAN_POINT('Origin',(-36.,-16.,0.));
#5873=CARTESIAN_POINT('',(-36.,16.,0.));
#5874=CARTESIAN_POINT('Origin',(40.,20.,0.));
#5875=CARTESIAN_POINT('',(40.,20.,0.));
#5876=CARTESIAN_POINT('Origin',(-40.,-20.,0.));
#5877=CARTESIAN_POINT('',(-40.,-20.,0.));
#5878=CARTESIAN_POINT('Origin',(0.,0.,0.));
#5879=CARTESIAN_POINT('',(0.,0.,0.));
#5880=CARTESIAN_POINT('Origin',(-19.,-19.,0.));
#5881=CARTESIAN_POINT('',(-19.,-20.,220.));
#5882=CARTESIAN_POINT('',(-20.,-19.,220.));
#5883=CARTESIAN_POINT('Origin',(-19.,-19.,220.));
#5884=CARTESIAN_POINT('',(-20.,-19.,0.));
#5885=CARTESIAN_POINT('',(-20.,-19.,0.));
#5886=CARTESIAN_POINT('',(-19.,-20.,0.));
#5887=CARTESIAN_POINT('Origin',(-19.,-19.,0.));
#5888=CARTESIAN_POINT('',(-19.,-20.,0.));
#5889=CARTESIAN_POINT('Origin',(-20.,20.,0.));
#5890=CARTESIAN_POINT('',(-20.,19.,220.));
#5891=CARTESIAN_POINT('',(-20.,20.,220.));
#5892=CARTESIAN_POINT('',(-20.,19.,0.));
#5893=CARTESIAN_POINT('',(-20.,19.,0.));
#5894=CARTESIAN_POINT('',(-20.,20.,0.));
#5895=CARTESIAN_POINT('Origin',(0.,0.,220.));
#5896=CARTESIAN_POINT('',(19.,-20.,220.));
#5897=CARTESIAN_POINT('',(-20.,-20.,220.));
#5898=CARTESIAN_POINT('',(20.,-19.,220.));
#5899=CARTESIAN_POINT('Origin',(19.,-19.,220.));
#5900=CARTESIAN_POINT('',(20.,19.,220.));
#5901=CARTESIAN_POINT('',(20.,-20.,220.));
#5902=CARTESIAN_POINT('',(19.,20.,220.));
#5903=CARTESIAN_POINT('Origin',(19.,19.,220.));
#5904=CARTESIAN_POINT('',(-19.,20.,220.));
#5905=CARTESIAN_POINT('',(20.,20.,220.));
#5906=CARTESIAN_POINT('Origin',(-19.,19.,220.));
#5907=CARTESIAN_POINT('',(-16.,-15.,220.));
#5908=CARTESIAN_POINT('',(-16.,15.,220.));
#5909=CARTESIAN_POINT('',(-16.,16.,220.));
#5910=CARTESIAN_POINT('',(-15.,16.,220.));
#5911=CARTESIAN_POINT('Origin',(-15.,15.,220.));
#5912=CARTESIAN_POINT('',(15.,16.,220.));
#5913=CARTESIAN_POINT('',(16.,16.,220.));
#5914=CARTESIAN_POINT('',(16.,15.,220.));
#5915=CARTESIAN_POINT('Origin',(15.,15.,220.));
#5916=CARTESIAN_POINT('',(16.,-15.,220.));
#5917=CARTESIAN_POINT('',(16.,-16.,220.));
#5918=CARTESIAN_POINT('',(15.,-16.,220.));
#5919=CARTESIAN_POINT('Origin',(15.,-15.,220.));
#5920=CARTESIAN_POINT('',(-15.,-16.,220.));
#5921=CARTESIAN_POINT('',(-16.,-16.,220.));
#5922=CARTESIAN_POINT('Origin',(-15.,-15.,220.));
#5923=CARTESIAN_POINT('Origin',(19.,-19.,0.));
#5924=CARTESIAN_POINT('',(19.,-20.,0.));
#5925=CARTESIAN_POINT('',(19.,-20.,0.));
#5926=CARTESIAN_POINT('',(20.,-19.,0.));
#5927=CARTESIAN_POINT('Origin',(19.,-19.,0.));
#5928=CARTESIAN_POINT('',(20.,-19.,0.));
#5929=CARTESIAN_POINT('Origin',(20.,-20.,0.));
#5930=CARTESIAN_POINT('',(20.,19.,0.));
#5931=CARTESIAN_POINT('',(20.,-20.,0.));
#5932=CARTESIAN_POINT('',(20.,19.,0.));
#5933=CARTESIAN_POINT('Origin',(19.,19.,0.));
#5934=CARTESIAN_POINT('',(19.,20.,0.));
#5935=CARTESIAN_POINT('Origin',(19.,19.,0.));
#5936=CARTESIAN_POINT('',(19.,20.,0.));
#5937=CARTESIAN_POINT('Origin',(-19.,19.,0.));
#5938=CARTESIAN_POINT('',(-19.,20.,0.));
#5939=CARTESIAN_POINT('',(-19.,20.,0.));
#5940=CARTESIAN_POINT('Origin',(-19.,19.,0.));
#5941=CARTESIAN_POINT('Origin',(-15.,15.,0.));
#5942=CARTESIAN_POINT('',(-16.,15.,0.));
#5943=CARTESIAN_POINT('',(-15.,16.,0.));
#5944=CARTESIAN_POINT('Origin',(-15.,15.,0.));
#5945=CARTESIAN_POINT('',(-15.,16.,0.));
#5946=CARTESIAN_POINT('',(-16.,15.,0.));
#5947=CARTESIAN_POINT('Origin',(-16.,16.,0.));
#5948=CARTESIAN_POINT('',(15.,16.,0.));
#5949=CARTESIAN_POINT('',(16.,16.,0.));
#5950=CARTESIAN_POINT('',(15.,16.,0.));
#5951=CARTESIAN_POINT('Origin',(15.,15.,0.));
#5952=CARTESIAN_POINT('',(16.,15.,0.));
#5953=CARTESIAN_POINT('Origin',(15.,15.,0.));
#5954=CARTESIAN_POINT('',(16.,15.,0.));
#5955=CARTESIAN_POINT('Origin',(16.,16.,0.));
#5956=CARTESIAN_POINT('',(16.,-15.,0.));
#5957=CARTESIAN_POINT('',(16.,-16.,0.));
#5958=CARTESIAN_POINT('',(16.,-15.,0.));
#5959=CARTESIAN_POINT('Origin',(15.,-15.,0.));
#5960=CARTESIAN_POINT('',(15.,-16.,0.));
#5961=CARTESIAN_POINT('Origin',(15.,-15.,0.));
#5962=CARTESIAN_POINT('',(15.,-16.,0.));
#5963=CARTESIAN_POINT('Origin',(16.,-16.,0.));
#5964=CARTESIAN_POINT('',(-15.,-16.,0.));
#5965=CARTESIAN_POINT('',(-16.,-16.,0.));
#5966=CARTESIAN_POINT('',(-15.,-16.,0.));
#5967=CARTESIAN_POINT('Origin',(-15.,-15.,0.));
#5968=CARTESIAN_POINT('',(-16.,-15.,0.));
#5969=CARTESIAN_POINT('Origin',(-15.,-15.,0.));
#5970=CARTESIAN_POINT('',(-16.,-15.,0.));
#5971=CARTESIAN_POINT('Origin',(-16.,-16.,0.));
#5972=CARTESIAN_POINT('',(-16.,16.,0.));
#5973=CARTESIAN_POINT('Origin',(20.,20.,0.));
#5974=CARTESIAN_POINT('',(20.,20.,0.));
#5975=CARTESIAN_POINT('Origin',(-20.,-20.,0.));
#5976=CARTESIAN_POINT('',(-20.,-20.,0.));
#5977=CARTESIAN_POINT('Origin',(0.,0.,0.));
#5978=CARTESIAN_POINT('',(0.,0.,0.));
#5979=CARTESIAN_POINT('Origin',(35.,-60.,6.));
#5980=CARTESIAN_POINT('',(28.,-60.,12.));
#5981=CARTESIAN_POINT('Origin',(35.,-60.,12.));
#5982=CARTESIAN_POINT('',(28.,-60.,0.));
#5983=CARTESIAN_POINT('',(28.,-60.,6.));
#5984=CARTESIAN_POINT('Origin',(35.,-60.,0.));
#5985=CARTESIAN_POINT('Origin',(-35.,-60.,6.));
#5986=CARTESIAN_POINT('',(-42.,-60.,12.));
#5987=CARTESIAN_POINT('Origin',(-35.,-60.,12.));
#5988=CARTESIAN_POINT('',(-42.,-60.,0.));
#5989=CARTESIAN_POINT('',(-42.,-60.,6.));
#5990=CARTESIAN_POINT('Origin',(-35.,-60.,0.));
#5991=CARTESIAN_POINT('Origin',(-35.,60.,6.));
#5992=CARTESIAN_POINT('',(-42.,60.,12.));
#5993=CARTESIAN_POINT('Origin',(-35.,60.,12.));
#5994=CARTESIAN_POINT('',(-42.,60.,0.));
#5995=CARTESIAN_POINT('',(-42.,60.,6.));
#5996=CARTESIAN_POINT('Origin',(-35.,60.,0.));
#5997=CARTESIAN_POINT('Origin',(35.,60.,6.));
#5998=CARTESIAN_POINT('',(28.,60.,12.));
#5999=CARTESIAN_POINT('Origin',(35.,60.,12.));
#6000=CARTESIAN_POINT('',(28.,60.,0.));
#6001=CARTESIAN_POINT('',(28.,60.,6.));
#6002=CARTESIAN_POINT('Origin',(35.,60.,0.));
#6003=CARTESIAN_POINT('Origin',(50.,86.,0.));
#6004=CARTESIAN_POINT('',(55.,86.,0.));
#6005=CARTESIAN_POINT('',(-50.,86.,0.));
#6006=CARTESIAN_POINT('',(25.,86.,0.));
#6007=CARTESIAN_POINT('',(-50.,86.,12.));
#6008=CARTESIAN_POINT('',(-50.,86.,0.));
#6009=CARTESIAN_POINT('',(55.,86.,12.));
#6010=CARTESIAN_POINT('',(25.,86.,12.));
#6011=CARTESIAN_POINT('',(55.,86.,0.));
#6012=CARTESIAN_POINT('Origin',(55.,-80.,0.));
#6013=CARTESIAN_POINT('',(55.,-86.,0.));
#6014=CARTESIAN_POINT('',(55.,-40.,0.));
#6015=CARTESIAN_POINT('',(55.,-86.,12.));
#6016=CARTESIAN_POINT('',(55.,-40.,12.));
#6017=CARTESIAN_POINT('',(55.,-86.,0.));
#6018=CARTESIAN_POINT('Origin',(-50.,-86.,0.));
#6019=CARTESIAN_POINT('',(-50.,-86.,0.));
#6020=CARTESIAN_POINT('',(-25.,-86.,0.));
#6021=CARTESIAN_POINT('',(-50.,-86.,12.));
#6022=CARTESIAN_POINT('',(-25.,-86.,12.));
#6023=CARTESIAN_POINT('',(-50.,-86.,0.));
#6024=CARTESIAN_POINT('Origin',(-50.,80.,0.));
#6025=CARTESIAN_POINT('',(-50.,80.,0.));
#6026=CARTESIAN_POINT('',(-50.,80.,12.));
#6027=CARTESIAN_POINT('Origin',(0.,0.,12.));
#6028=CARTESIAN_POINT('Origin',(0.,0.,0.));
#6029=CARTESIAN_POINT('',(0.,0.,0.));
#6030=CARTESIAN_POINT('Origin',(35.,-60.,4.));
#6031=CARTESIAN_POINT('',(28.,-60.,8.));
#6032=CARTESIAN_POINT('Origin',(35.,-60.,8.));
#6033=CARTESIAN_POINT('',(28.,-60.,0.));
#6034=CARTESIAN_POINT('',(28.,-60.,4.));
#6035=CARTESIAN_POINT('Origin',(35.,-60.,0.));
#6036=CARTESIAN_POINT('Origin',(-35.,-60.,4.));
#6037=CARTESIAN_POINT('',(-42.,-60.,8.));
#6038=CARTESIAN_POINT('Origin',(-35.,-60.,8.));
#6039=CARTESIAN_POINT('',(-42.,-60.,0.));
#6040=CARTESIAN_POINT('',(-42.,-60.,4.));
#6041=CARTESIAN_POINT('Origin',(-35.,-60.,0.));
#6042=CARTESIAN_POINT('Origin',(-35.,60.,4.));
#6043=CARTESIAN_POINT('',(-42.,60.,8.));
#6044=CARTESIAN_POINT('Origin',(-35.,60.,8.));
#6045=CARTESIAN_POINT('',(-42.,60.,0.));
#6046=CARTESIAN_POINT('',(-42.,60.,4.));
#6047=CARTESIAN_POINT('Origin',(-35.,60.,0.));
#6048=CARTESIAN_POINT('Origin',(35.,60.,4.));
#6049=CARTESIAN_POINT('',(28.,60.,8.));
#6050=CARTESIAN_POINT('Origin',(35.,60.,8.));
#6051=CARTESIAN_POINT('',(28.,60.,0.));
#6052=CARTESIAN_POINT('',(28.,60.,4.));
#6053=CARTESIAN_POINT('Origin',(35.,60.,0.));
#6054=CARTESIAN_POINT('Origin',(50.,86.,0.));
#6055=CARTESIAN_POINT('',(55.,86.,0.));
#6056=CARTESIAN_POINT('',(-50.,86.,0.));
#6057=CARTESIAN_POINT('',(25.,86.,0.));
#6058=CARTESIAN_POINT('',(-50.,86.,8.));
#6059=CARTESIAN_POINT('',(-50.,86.,0.));
#6060=CARTESIAN_POINT('',(55.,86.,8.));
#6061=CARTESIAN_POINT('',(25.,86.,8.));
#6062=CARTESIAN_POINT('',(55.,86.,0.));
#6063=CARTESIAN_POINT('Origin',(55.,-80.,0.));
#6064=CARTESIAN_POINT('',(55.,-86.,0.));
#6065=CARTESIAN_POINT('',(55.,-40.,0.));
#6066=CARTESIAN_POINT('',(55.,-86.,8.));
#6067=CARTESIAN_POINT('',(55.,-40.,8.));
#6068=CARTESIAN_POINT('',(55.,-86.,0.));
#6069=CARTESIAN_POINT('Origin',(-50.,-86.,0.));
#6070=CARTESIAN_POINT('',(-50.,-86.,0.));
#6071=CARTESIAN_POINT('',(-25.,-86.,0.));
#6072=CARTESIAN_POINT('',(-50.,-86.,8.));
#6073=CARTESIAN_POINT('',(-25.,-86.,8.));
#6074=CARTESIAN_POINT('',(-50.,-86.,0.));
#6075=CARTESIAN_POINT('Origin',(-50.,80.,0.));
#6076=CARTESIAN_POINT('',(-50.,80.,0.));
#6077=CARTESIAN_POINT('',(-50.,80.,8.));
#6078=CARTESIAN_POINT('Origin',(0.,0.,8.));
#6079=CARTESIAN_POINT('Origin',(0.,0.,0.));
#6080=CARTESIAN_POINT('',(0.,0.,0.));
#6081=CARTESIAN_POINT('Origin',(40.,20.,0.));
#6082=CARTESIAN_POINT('',(40.,20.,0.));
#6083=CARTESIAN_POINT('',(-40.,20.,0.));
#6084=CARTESIAN_POINT('',(40.,20.,0.));
#6085=CARTESIAN_POINT('',(-40.,20.,4.));
#6086=CARTESIAN_POINT('',(-40.,20.,0.));
#6087=CARTESIAN_POINT('',(40.,20.,4.));
#6088=CARTESIAN_POINT('',(40.,20.,4.));
#6089=CARTESIAN_POINT('',(40.,20.,0.));
#6090=CARTESIAN_POINT('Origin',(40.,-20.,0.));
#6091=CARTESIAN_POINT('',(40.,-20.,0.));
#6092=CARTESIAN_POINT('',(40.,-20.,0.));
#6093=CARTESIAN_POINT('',(40.,-20.,4.));
#6094=CARTESIAN_POINT('',(40.,-20.,4.));
#6095=CARTESIAN_POINT('',(40.,-20.,0.));
#6096=CARTESIAN_POINT('Origin',(-40.,-20.,0.));
#6097=CARTESIAN_POINT('',(-40.,-20.,0.));
#6098=CARTESIAN_POINT('',(-40.,-20.,0.));
#6099=CARTESIAN_POINT('',(-40.,-20.,4.));
#6100=CARTESIAN_POINT('',(-40.,-20.,4.));
#6101=CARTESIAN_POINT('',(-40.,-20.,0.));
#6102=CARTESIAN_POINT('Origin',(-40.,20.,0.));
#6103=CARTESIAN_POINT('',(-40.,20.,0.));
#6104=CARTESIAN_POINT('',(-40.,20.,4.));
#6105=CARTESIAN_POINT('Origin',(0.,0.,4.));
#6106=CARTESIAN_POINT('Origin',(0.,0.,0.));
#6107=CARTESIAN_POINT('',(0.,0.,0.));
#6108=CARTESIAN_POINT('Origin',(5.,30.,0.));
#6109=CARTESIAN_POINT('',(5.,30.,0.));
#6110=CARTESIAN_POINT('',(-5.,30.,0.));
#6111=CARTESIAN_POINT('',(5.,30.,0.));
#6112=CARTESIAN_POINT('',(-5.,30.,20.));
#6113=CARTESIAN_POINT('',(-5.,30.,0.));
#6114=CARTESIAN_POINT('',(5.,30.,20.));
#6115=CARTESIAN_POINT('',(5.,30.,20.));
#6116=CARTESIAN_POINT('',(5.,30.,0.));
#6117=CARTESIAN_POINT('Origin',(5.,-30.,0.));
#6118=CARTESIAN_POINT('',(5.,-30.,0.));
#6119=CARTESIAN_POINT('',(5.,-30.,0.));
#6120=CARTESIAN_POINT('',(5.,-30.,20.));
#6121=CARTESIAN_POINT('',(5.,-30.,20.));
#6122=CARTESIAN_POINT('',(5.,-30.,0.));
#6123=CARTESIAN_POINT('Origin',(-5.,-30.,0.));
#6124=CARTESIAN_POINT('',(-5.,-30.,0.));
#6125=CARTESIAN_POINT('',(-5.,-30.,0.));
#6126=CARTESIAN_POINT('',(-5.,-30.,20.));
#6127=CARTESIAN_POINT('',(-5.,-30.,20.));
#6128=CARTESIAN_POINT('',(-5.,-30.,0.));
#6129=CARTESIAN_POINT('Origin',(-5.,30.,0.));
#6130=CARTESIAN_POINT('',(-5.,30.,0.));
#6131=CARTESIAN_POINT('',(-5.,30.,20.));
#6132=CARTESIAN_POINT('Origin',(0.,0.,20.));
#6133=CARTESIAN_POINT('Origin',(0.,0.,0.));
#6134=CARTESIAN_POINT('',(0.,0.,0.));
#6135=CARTESIAN_POINT('Origin',(30.,0.,225.));
#6136=CARTESIAN_POINT('',(30.,4.,219.));
#6137=CARTESIAN_POINT('Origin',(30.,4.,225.));
#6138=CARTESIAN_POINT('',(30.,-4.,219.));
#6139=CARTESIAN_POINT('',(30.,0.,219.));
#6140=CARTESIAN_POINT('Origin',(30.,-4.,225.));
#6141=CARTESIAN_POINT('Origin',(-30.,0.,225.));
#6142=CARTESIAN_POINT('',(-30.,4.,219.));
#6143=CARTESIAN_POINT('Origin',(-30.,4.,225.));
#6144=CARTESIAN_POINT('',(-30.,-4.,219.));
#6145=CARTESIAN_POINT('',(-30.,0.,219.));
#6146=CARTESIAN_POINT('Origin',(-30.,-4.,225.));
#6147=CARTESIAN_POINT('Origin',(-30.,0.,295.));
#6148=CARTESIAN_POINT('',(-30.,4.,289.));
#6149=CARTESIAN_POINT('Origin',(-30.,4.,295.));
#6150=CARTESIAN_POINT('',(-30.,-4.,289.));
#6151=CARTESIAN_POINT('',(-30.,0.,289.));
#6152=CARTESIAN_POINT('Origin',(-30.,-4.,295.));
#6153=CARTESIAN_POINT('Origin',(30.,0.,295.));
#6154=CARTESIAN_POINT('',(30.,4.,289.));
#6155=CARTESIAN_POINT('Origin',(30.,4.,295.));
#6156=CARTESIAN_POINT('',(30.,-4.,289.));
#6157=CARTESIAN_POINT('',(30.,0.,289.));
#6158=CARTESIAN_POINT('Origin',(30.,-4.,295.));
#6159=CARTESIAN_POINT('Origin',(60.,4.,200.));
#6160=CARTESIAN_POINT('',(60.,4.,200.));
#6161=CARTESIAN_POINT('',(-60.,4.,200.));
#6162=CARTESIAN_POINT('',(60.,4.,200.));
#6163=CARTESIAN_POINT('',(-60.,4.,320.));
#6164=CARTESIAN_POINT('',(-60.,4.,200.));
#6165=CARTESIAN_POINT('',(60.,4.,320.));
#6166=CARTESIAN_POINT('',(60.,4.,320.));
#6167=CARTESIAN_POINT('',(60.,4.,200.));
#6168=CARTESIAN_POINT('Origin',(60.,-4.,200.));
#6169=CARTESIAN_POINT('',(60.,-4.,200.));
#6170=CARTESIAN_POINT('',(60.,-4.,200.));
#6171=CARTESIAN_POINT('',(60.,-4.,320.));
#6172=CARTESIAN_POINT('',(60.,-4.,320.));
#6173=CARTESIAN_POINT('',(60.,-4.,200.));
#6174=CARTESIAN_POINT('Origin',(-60.,-4.,200.));
#6175=CARTESIAN_POINT('',(-60.,-4.,200.));
#6176=CARTESIAN_POINT('',(-60.,-4.,200.));
#6177=CARTESIAN_POINT('',(-60.,-4.,320.));
#6178=CARTESIAN_POINT('',(-60.,-4.,320.));
#6179=CARTESIAN_POINT('',(-60.,-4.,200.));
#6180=CARTESIAN_POINT('Origin',(-60.,4.,200.));
#6181=CARTESIAN_POINT('',(-60.,4.,200.));
#6182=CARTESIAN_POINT('',(-60.,4.,320.));
#6183=CARTESIAN_POINT('Origin',(0.,0.,320.));
#6184=CARTESIAN_POINT('Origin',(0.,0.,200.));
#6185=CARTESIAN_POINT('',(0.,0.,0.));
#6186=CARTESIAN_POINT('Origin',(40.,30.,5.));
#6187=CARTESIAN_POINT('',(37.4865492426837,30.0006055736961,0.387416697508023));
#6188=CARTESIAN_POINT('',(37.4843813836159,29.9964988963182,0.112583302491979));
#6189=CARTESIAN_POINT('',(37.4825,30.,5.));
#6190=CARTESIAN_POINT('',(38.086534003335,31.635987203375,0.));
#6191=CARTESIAN_POINT('Ctrl Pts',(37.4843813836159,29.9964988963182,0.112583302491979));
#6192=CARTESIAN_POINT('Ctrl Pts',(37.4896308378643,30.5890976659027,0.0750555349946511));
#6193=CARTESIAN_POINT('Ctrl Pts',(37.700778171916,31.1848035603044,0.0375277674973235));
#6194=CARTESIAN_POINT('Ctrl Pts',(38.086534003335,31.635987203375,-4.44089209850063E-15));
#6195=CARTESIAN_POINT('',(41.9171065683076,31.6387569269747,-6.03363952037314E-16));
#6196=CARTESIAN_POINT('Origin',(40.,30.,0.));
#6197=CARTESIAN_POINT('Ctrl Pts',(41.9171095224698,31.6387591744824,-4.02677955152094E-16));
#6198=CARTESIAN_POINT('Ctrl Pts',(41.3863013821206,32.2578627143831,0.0517824693358733));
#6199=CARTESIAN_POINT('Ctrl Pts',(40.5267002275034,32.5973566946348,0.103564938671747));
#6200=CARTESIAN_POINT('Ctrl Pts',(39.7163628727442,32.5055173392451,0.15534740800762));
#6201=CARTESIAN_POINT('Ctrl Pts',(38.8880955008986,32.4116458904295,0.208275647749515));
#6202=CARTESIAN_POINT('Ctrl Pts',(38.1112961294035,31.867142043505,0.26120388749141));
#6203=CARTESIAN_POINT('Ctrl Pts',(37.7410321515366,31.1206209684195,0.314132127233305));
#6204=CARTESIAN_POINT('Ctrl Pts',(37.5701426815768,30.7760759992598,0.338560317324878));
#6205=CARTESIAN_POINT('Ctrl Pts',(37.485850848764,30.3884985785696,0.36298850741645));
#6206=CARTESIAN_POINT('Ctrl Pts',(37.4865492426837,30.0006055736961,0.387416697508023));
#6207=CARTESIAN_POINT('Origin',(40.,30.,5.));
#6208=CARTESIAN_POINT('',(37.4826513052474,29.9976965354932,1.38741669750802));
#6209=CARTESIAN_POINT('',(37.4783311322817,30.0001213195654,1.11258330249198));
#6210=CARTESIAN_POINT('',(37.4825,30.,5.));
#6211=CARTESIAN_POINT('Ctrl Pts',(37.4783311322817,30.0001213195654,1.11258330249198));
#6212=CARTESIAN_POINT('Ctrl Pts',(37.4783275808006,30.0058437240052,1.11221987985458));
#6213=CARTESIAN_POINT('Ctrl Pts',(37.4783453684107,30.0115661037913,1.11185645721718));
#6214=CARTESIAN_POINT('Ctrl Pts',(37.4783845615425,30.0172883349493,1.11149303457978));
#6215=CARTESIAN_POINT('Ctrl Pts',(37.4840925809837,30.8506641113011,1.05856479483789));
#6216=CARTESIAN_POINT('Ctrl Pts',(37.9438224654611,31.6808874105992,1.00563655509599));
#6217=CARTESIAN_POINT('Ctrl Pts',(38.6471444516464,32.1280310844825,0.952708315354099));
#6218=CARTESIAN_POINT('Ctrl Pts',(39.3504664378318,32.5751747583658,0.899780075612205));
#6219=CARTESIAN_POINT('Ctrl Pts',(40.2973805257251,32.6392388068343,0.84685183587031));
#6220=CARTESIAN_POINT('Ctrl Pts',(41.0544290556679,32.2906973355318,0.793923596128415));
#6221=CARTESIAN_POINT('Ctrl Pts',(41.8114775856107,31.9421558642292,0.740995356386521));
#6222=CARTESIAN_POINT('Ctrl Pts',(42.378660557603,31.1810088731556,0.688067116644628));
#6223=CARTESIAN_POINT('Ctrl Pts',(42.496385640448,30.3560668613964,0.635138876902733));
#6224=CARTESIAN_POINT('Ctrl Pts',(42.6141107232931,29.5311248496373,0.582210637160839));
#6225=CARTESIAN_POINT('Ctrl Pts',(42.282377916991,28.6423878171925,0.529282397418944));
#6226=CARTESIAN_POINT('Ctrl Pts',(41.6529742937847,28.0958630035297,0.47635415767705));
#6227=CARTESIAN_POINT('Ctrl Pts',(41.0235706705784,27.5493381898668,0.423425917935155));
#6228=CARTESIAN_POINT('Ctrl Pts',(40.0964962304679,27.3450255949858,0.370497678193261));
#6229=CARTESIAN_POINT('Ctrl Pts',(39.2962221198814,27.5780866114451,0.317569438451365));
#6230=CARTESIAN_POINT('Ctrl Pts',(38.495948009295,27.8111476279043,0.264641198709472));
#6231=CARTESIAN_POINT('Ctrl Pts',(37.8224742282327,28.4815822557037,0.211712958967577));
#6232=CARTESIAN_POINT('Ctrl Pts',(37.5841055938905,29.2787075728659,0.158784719225683));
#6233=CARTESIAN_POINT('Ctrl Pts',(37.5147477320938,29.5106462578148,0.143384246981115));
#6234=CARTESIAN_POINT('Ctrl Pts',(37.4822271367784,29.7533109447887,0.127983774736547));
#6235=CARTESIAN_POINT('Ctrl Pts',(37.4843813836159,29.9964988963182,0.112583302491979));
#6236=CARTESIAN_POINT('Ctrl Pts',(37.4865492426837,30.0006055736961,0.387416697508023));
#6237=CARTESIAN_POINT('Ctrl Pts',(37.4873640497288,29.548055881866,0.415916747158346));
#6238=CARTESIAN_POINT('Ctrl Pts',(37.6038640135046,29.0950766299899,0.444416796808668));
#6239=CARTESIAN_POINT('Ctrl Pts',(37.8334964929258,28.7095041526117,0.472916846458991));
#6240=CARTESIAN_POINT('Ctrl Pts',(38.2599533964209,27.9934467151356,0.525845086200884));
#6241=CARTESIAN_POINT('Ctrl Pts',(39.0765957876499,27.5098701434296,0.578773325942778));
#6242=CARTESIAN_POINT('Ctrl Pts',(39.9094857112398,27.479971270026,0.631701565684672));
#6243=CARTESIAN_POINT('Ctrl Pts',(40.7423756348297,27.4500723966223,0.684629805426567));
#6244=CARTESIAN_POINT('Ctrl Pts',(41.5915130907804,27.8738512215209,0.737558045168462));
#6245=CARTESIAN_POINT('Ctrl Pts',(42.0682758200043,28.5574047494562,0.790486284910356));
#6246=CARTESIAN_POINT('Ctrl Pts',(42.5450385492282,29.2409582773914,0.843414524652251));
#6247=CARTESIAN_POINT('Ctrl Pts',(42.6494265517252,30.1842865083634,0.896342764394145));
#6248=CARTESIAN_POINT('Ctrl Pts',(42.333625344339,30.9555495584931,0.949271004136039));
#6249=CARTESIAN_POINT('Ctrl Pts',(42.0178241369527,31.7268126086228,1.00219924387793));
#6250=CARTESIAN_POINT('Ctrl Pts',(41.2818337196832,32.3260104779102,1.05512748361983));
#6251=CARTESIAN_POINT('Ctrl Pts',(40.4625635148939,32.4788849033583,1.10805572336172));
#6252=CARTESIAN_POINT('Ctrl Pts',(39.6432933101047,32.6317593288063,1.16098396310362));
#6253=CARTESIAN_POINT('Ctrl Pts',(38.7407433177957,32.3383103104151,1.21391220284551));
#6254=CARTESIAN_POINT('Ctrl Pts',(38.1680403886987,31.7328518944262,1.26684044258741));
#6255=CARTESIAN_POINT('Ctrl Pts',(37.733147316435,31.273085308157,1.30703252756095));
#6256=CARTESIAN_POINT('Ctrl Pts',(37.488457870222,30.6334010406233,1.34722461253449));
#6257=CARTESIAN_POINT('Ctrl Pts',(37.4826513052474,29.9976965354932,1.38741669750802));
#6258=CARTESIAN_POINT('Origin',(40.,30.,5.));
#6259=CARTESIAN_POINT('',(37.4786864827572,30.000865351545,2.38741669750803));
#6260=CARTESIAN_POINT('',(37.4841918288605,30.0021290961335,2.11258330249198));
#6261=CARTESIAN_POINT('',(37.4825,30.,5.));
#6262=CARTESIAN_POINT('Ctrl Pts',(37.4841918288605,30.0021290961335,2.11258330249198));
#6263=CARTESIAN_POINT('Ctrl Pts',(37.4821415438194,30.257605834553,2.09645598497262));
#6264=CARTESIAN_POINT('Ctrl Pts',(37.517933068672,30.5125215673247,2.08032866745325));
#6265=CARTESIAN_POINT('Ctrl Pts',(37.5939458442133,30.7548191659607,2.06420134993388));
#6266=CARTESIAN_POINT('Ctrl Pts',(37.8434121551767,31.5500156004633,2.01127311019199));
#6267=CARTESIAN_POINT('Ctrl Pts',(38.5260961730752,32.2093038013217,1.9583448704501));
#6268=CARTESIAN_POINT('Ctrl Pts',(39.3295050503994,32.4309016291222,1.9054166307082));
#6269=CARTESIAN_POINT('Ctrl Pts',(40.1329139277237,32.6524994569227,1.85248839096631));
#6270=CARTESIAN_POINT('Ctrl Pts',(41.0570476644737,32.4364069116652,1.79956015122441));
#6271=CARTESIAN_POINT('Ctrl Pts',(41.6788914300393,31.8815353981424,1.74663191148252));
#6272=CARTESIAN_POINT('Ctrl Pts',(42.300735195605,31.3266638846196,1.69370367174062));
#6273=CARTESIAN_POINT('Ctrl Pts',(42.6202889899864,30.4330134028314,1.64077543199873));
#6274=CARTESIAN_POINT('Ctrl Pts',(42.4912801935499,29.6096514151861,1.58784719225683));
#6275=CARTESIAN_POINT('Ctrl Pts',(42.3622713971135,28.7862894275408,1.53491895251494));
#6276=CARTESIAN_POINT('Ctrl Pts',(41.7847000098592,28.0332159340385,1.48199071277304));
#6277=CARTESIAN_POINT('Ctrl Pts',(41.0229435846798,27.6951314558291,1.42906247303115));
#6278=CARTESIAN_POINT('Ctrl Pts',(40.2611871595004,27.3570469776196,1.37613423328926));
#6279=CARTESIAN_POINT('Ctrl Pts',(39.315245696396,27.4339515147031,1.32320599354736));
#6280=CARTESIAN_POINT('Ctrl Pts',(38.6181180420463,27.8906679099476,1.27027775380547));
#6281=CARTESIAN_POINT('Ctrl Pts',(37.9257770946035,28.3442483407671,1.21771293670097));
#6282=CARTESIAN_POINT('Ctrl Pts',(37.478844812322,29.1724427111836,1.16514811959648));
#6283=CARTESIAN_POINT('Ctrl Pts',(37.4783311322817,30.0001213195654,1.11258330249198));
#6284=CARTESIAN_POINT('Ctrl Pts',(37.4826513052474,29.9976965354932,1.38741669750802));
#6285=CARTESIAN_POINT('Ctrl Pts',(37.4808113083864,29.7962531177255,1.40015285227638));
#6286=CARTESIAN_POINT('Ctrl Pts',(37.502958569874,29.5952093250312,1.41288900704473));
#6287=CARTESIAN_POINT('Ctrl Pts',(37.5506420393601,29.4004166824566,1.42562516181309));
#6288=CARTESIAN_POINT('Ctrl Pts',(37.7488024850036,28.5909077000624,1.47855340155498));
#6289=CARTESIAN_POINT('Ctrl Pts',(38.3879792421759,27.8893575488604,1.53148164129688));
#6290=CARTESIAN_POINT('Ctrl Pts',(39.1755924364077,27.6168925555489,1.58440988103877));
#6291=CARTESIAN_POINT('Ctrl Pts',(39.9632056306395,27.3444275622373,1.63733812078067));
#6292=CARTESIAN_POINT('Ctrl Pts',(40.8992552619309,27.5010477268163,1.69026636052256));
#6293=CARTESIAN_POINT('Ctrl Pts',(41.5552733407625,28.0150626943082,1.74319460026446));
#6294=CARTESIAN_POINT('Ctrl Pts',(42.2112914195941,28.5290776618002,1.79612284000635));
#6295=CARTESIAN_POINT('Ctrl Pts',(42.5872779459659,29.4004874322051,1.84905107974825));
#6296=CARTESIAN_POINT('Ctrl Pts',(42.5111276934142,30.2304107639936,1.90197931949014));
#6297=CARTESIAN_POINT('Ctrl Pts',(42.4349774408626,31.060334095782,1.95490755923204));
#6298=CARTESIAN_POINT('Ctrl Pts',(41.9066904093874,31.848770988954,2.00783579897393));
#6299=CARTESIAN_POINT('Ctrl Pts',(41.1680858742699,32.23482127651,2.06076403871582));
#6300=CARTESIAN_POINT('Ctrl Pts',(40.4294813391524,32.6208715640661,2.11369227845772));
#6301=CARTESIAN_POINT('Ctrl Pts',(39.4805593003925,32.6045352460063,2.16662051819961));
#6302=CARTESIAN_POINT('Ctrl Pts',(38.7556808583415,32.1932899824628,2.21954875794151));
#6303=CARTESIAN_POINT('Ctrl Pts',(38.0308024162905,31.7820447189193,2.2724769976834));
#6304=CARTESIAN_POINT('Ctrl Pts',(37.5299675709483,30.9758905098923,2.3254052374253));
#6305=CARTESIAN_POINT('Ctrl Pts',(37.482429398745,30.1438378634159,2.37833347716719));
#6306=CARTESIAN_POINT('Ctrl Pts',(37.4797099954244,30.0962406036797,2.3813612172808));
#6307=CARTESIAN_POINT('Ctrl Pts',(37.4784739461469,30.0485585946962,2.38438895739441));
#6308=CARTESIAN_POINT('Ctrl Pts',(37.4786864827572,30.000865351545,2.38741669750803));
#6309=CARTESIAN_POINT('Origin',(40.,30.,5.));
#6310=CARTESIAN_POINT('',(37.4852129709663,30.0017637215755,3.38741669750803));
#6311=CARTESIAN_POINT('',(37.485883012183,29.9986698324052,3.11258330249198));
#6312=CARTESIAN_POINT('',(37.4825,30.,5.));
#6313=CARTESIAN_POINT('Ctrl Pts',(37.485883012183,29.9986698324052,3.11258330249198));
#6314=CARTESIAN_POINT('Ctrl Pts',(37.4883076973175,30.504721507644,3.08069209009065));
#6315=CARTESIAN_POINT('Ctrl Pts',(37.636377858221,31.0120786438038,3.04880087768932));
#6316=CARTESIAN_POINT('Ctrl Pts',(37.920388915981,31.4262068815774,3.01690966528799));
#6317=CARTESIAN_POINT('Ctrl Pts',(38.3917477707431,32.1135146695953,2.96398142554609));
#6318=CARTESIAN_POINT('Ctrl Pts',(39.2375472597066,32.5440293317411,2.9110531858042));
#6319=CARTESIAN_POINT('Ctrl Pts',(40.0706296546987,32.5206863623676,2.8581249460623));
#6320=CARTESIAN_POINT('Ctrl Pts',(40.9037120496908,32.497343392994,2.80519670632041));
#6321=CARTESIAN_POINT('Ctrl Pts',(41.7240773507114,32.0201427921011,2.75226846657851));
#6322=CARTESIAN_POINT('Ctrl Pts',(42.1562101132269,31.3075191431985,2.69934022683662));
#6323=CARTESIAN_POINT('Ctrl Pts',(42.5883428757425,30.594895494296,2.64641198709473));
#6324=CARTESIAN_POINT('Ctrl Pts',(42.6322430997529,29.6468487973838,2.59348374735283));
#6325=CARTESIAN_POINT('Ctrl Pts',(42.2678158280527,28.8973396974625,2.54055550761094));
#6326=CARTESIAN_POINT('Ctrl Pts',(41.9033885563526,28.1478305975413,2.48762726786904));
#6327=CARTESIAN_POINT('Ctrl Pts',(41.1306337889419,27.5968590946111,2.43469902812715));
#6328=CARTESIAN_POINT('Ctrl Pts',(40.3032736225135,27.4966276437265,2.38177078838525));
#6329=CARTESIAN_POINT('Ctrl Pts',(39.4759134560852,27.3963961928419,2.32884254864336));
#6330=CARTESIAN_POINT('Ctrl Pts',(38.5939478906392,27.746904794003,2.27591430890146));
#6331=CARTESIAN_POINT('Ctrl Pts',(38.0610894099303,28.387711428657,2.22298606915957));
#6332=CARTESIAN_POINT('Ctrl Pts',(37.6905937425927,28.8332632784178,2.18618514693704));
#6333=CARTESIAN_POINT('Ctrl Pts',(37.4888703738348,29.419156784157,2.14938422471451));
#6334=CARTESIAN_POINT('Ctrl Pts',(37.4841918288605,30.0021290961335,2.11258330249198));
#6335=CARTESIAN_POINT('Ctrl Pts',(37.4786864827572,30.000865351545,2.38741669750803));
#6336=CARTESIAN_POINT('Ctrl Pts',(37.4821893207308,29.2148280521618,2.43731719713631));
#6337=CARTESIAN_POINT('Ctrl Pts',(37.8791668909914,28.4257392519124,2.48721769676459));
#6338=CARTESIAN_POINT('Ctrl Pts',(38.5139722677769,27.9627045952532,2.53711819639288));
#6339=CARTESIAN_POINT('Ctrl Pts',(39.1872948080768,27.4715750574926,2.59004643613477));
#6340=CARTESIAN_POINT('Ctrl Pts',(40.128181387741,27.347267065897,2.64297467587667));
#6341=CARTESIAN_POINT('Ctrl Pts',(40.9059489619732,27.6466815962724,2.69590291561856));
#6342=CARTESIAN_POINT('Ctrl Pts',(41.6837165362054,27.9460961266478,2.74883115536045));
#6343=CARTESIAN_POINT('Ctrl Pts',(42.2983651050056,28.669233178994,2.80175939510235));
#6344=CARTESIAN_POINT('Ctrl Pts',(42.4685443548906,29.4850827307125,2.85468763484424));
#6345=CARTESIAN_POINT('Ctrl Pts',(42.6387236047757,30.300932282431,2.90761587458614));
#6346=CARTESIAN_POINT('Ctrl Pts',(42.3644335357456,31.2094943335216,2.96054411432803));
#6347=CARTESIAN_POINT('Ctrl Pts',(41.7712281653103,31.7948821143088,3.01347235406993));
#6348=CARTESIAN_POINT('Ctrl Pts',(41.1780227948749,32.3802698950961,3.06640059381182));
#6349=CARTESIAN_POINT('Ctrl Pts',(40.2659021230343,32.6424834055799,3.11932883355372));
#6350=CARTESIAN_POINT('Ctrl Pts',(39.4523818516077,32.4614965746811,3.17225707329561));
#6351=CARTESIAN_POINT('Ctrl Pts',(38.6388615801811,32.2805097437823,3.22518531303751));
#6352=CARTESIAN_POINT('Ctrl Pts',(37.9239417091685,31.6563225715008,3.2781135527794));
#6353=CARTESIAN_POINT('Ctrl Pts',(37.6348709055651,30.8746515816341,3.33104179252129));
#6354=CARTESIAN_POINT('Ctrl Pts',(37.5322392470085,30.597127220351,3.34983342751687));
#6355=CARTESIAN_POINT('Ctrl Pts',(37.4832872705902,30.299751503466,3.36862506251245));
#6356=CARTESIAN_POINT('Ctrl Pts',(37.4852129709663,30.0017637215755,3.38741669750803));
#6357=CARTESIAN_POINT('Origin',(40.,30.,5.));
#6358=CARTESIAN_POINT('',(37.4850671861185,29.9981671622093,4.38741669750803));
#6359=CARTESIAN_POINT('',(37.4793386265487,29.9985765177349,4.11258330249198));
#6360=CARTESIAN_POINT('',(37.4825,30.,5.));
#6361=CARTESIAN_POINT('Ctrl Pts',(37.4793386265487,29.9985765177349,4.11258330249198));
#6362=CARTESIAN_POINT('Ctrl Pts',(37.4844207242438,30.7497576670511,4.06492819520868));
#6363=CARTESIAN_POINT('Ctrl Pts',(37.8421139480676,31.5051391927042,4.01727308792539));
#6364=CARTESIAN_POINT('Ctrl Pts',(38.4291013453193,31.9725936575687,3.96961798064209));
#6365=CARTESIAN_POINT('Ctrl Pts',(39.0810400662316,32.4917728892444,3.91668974090019));
#6366=CARTESIAN_POINT('Ctrl Pts',(40.0158241202065,32.6557803161201,3.8637615011583));
#6367=CARTESIAN_POINT('Ctrl Pts',(40.8055638275036,32.3895428935737,3.8108332614164));
#6368=CARTESIAN_POINT('Ctrl Pts',(41.5953035348006,32.1233054710273,3.75790502167451));
#6369=CARTESIAN_POINT('Ctrl Pts',(42.2399988954197,31.4268231990587,3.70497678193261));
#6370=CARTESIAN_POINT('Ctrl Pts',(42.4445459328977,30.6189050842116,3.65204854219072));
#6371=CARTESIAN_POINT('Ctrl Pts',(42.6490929703756,29.8109869693645,3.59912030244883));
#6372=CARTESIAN_POINT('Ctrl Pts',(42.4134916847125,28.8916330116387,3.54619206270693));
#6373=CARTESIAN_POINT('Ctrl Pts',(41.8455866185718,28.2816698932712,3.49326382296504));
#6374=CARTESIAN_POINT('Ctrl Pts',(41.2776815524311,27.6717067749037,3.44033558322314));
#6375=CARTESIAN_POINT('Ctrl Pts',(40.377472705813,27.3711344958944,3.38740734348125));
#6376=CARTESIAN_POINT('Ctrl Pts',(39.5570232426543,27.5175375312054,3.33447910373935));
#6377=CARTESIAN_POINT('Ctrl Pts',(38.7365737794957,27.6639405665165,3.28155086399746));
#6378=CARTESIAN_POINT('Ctrl Pts',(37.9958836997965,28.2573189161479,3.22862262425556));
#6379=CARTESIAN_POINT('Ctrl Pts',(37.6739977702273,29.0260585479087,3.17569438451367));
#6380=CARTESIAN_POINT('Ctrl Pts',(37.5460599598276,29.3316042590449,3.15465735717311));
#6381=CARTESIAN_POINT('Ctrl Pts',(37.4842835694643,29.6648530181128,3.13362032983254));
#6382=CARTESIAN_POINT('Ctrl Pts',(37.485883012183,29.9986698324052,3.11258330249198));
#6383=CARTESIAN_POINT('Ctrl Pts',(37.4852129709663,30.0017637215755,3.38741669750803));
#6384=CARTESIAN_POINT('Ctrl Pts',(37.4887111696391,29.4604435473585,3.42155330225434));
#6385=CARTESIAN_POINT('Ctrl Pts',(37.6601047626962,28.9171035699204,3.45568990700066));
#6386=CARTESIAN_POINT('Ctrl Pts',(37.9825965759643,28.4870775147433,3.48982651174698));
#6387=CARTESIAN_POINT('Ctrl Pts',(38.4826147861612,27.8203292451712,3.54275475148887));
#6388=CARTESIAN_POINT('Ctrl Pts',(39.3458729427491,27.4259875134789,3.59568299123076));
#6389=CARTESIAN_POINT('Ctrl Pts',(40.1772217549583,27.4845589905516,3.64861123097266));
#6390=CARTESIAN_POINT('Ctrl Pts',(41.0085705671675,27.5431304676243,3.70153947071455));
#6391=CARTESIAN_POINT('Ctrl Pts',(41.8080100349979,28.0546151534619,3.75446771045645));
#6392=CARTESIAN_POINT('Ctrl Pts',(42.209603344971,28.7848851576249,3.80739595019834));
#6393=CARTESIAN_POINT('Ctrl Pts',(42.6111966549441,29.5151551617878,3.86032418994024));
#6394=CARTESIAN_POINT('Ctrl Pts',(42.6149438070599,30.464210484276,3.91325242968213));
#6395=CARTESIAN_POINT('Ctrl Pts',(42.2191295734494,31.1976288901078,3.96618066942403));
#6396=CARTESIAN_POINT('Ctrl Pts',(41.8233153398388,31.9310472959396,4.01910890916592));
#6397=CARTESIAN_POINT('Ctrl Pts',(41.0279397205019,32.448828785115,4.07203714890782));
#6398=CARTESIAN_POINT('Ctrl Pts',(40.1970793356802,32.5139631575899,4.12496538864971));
#6399=CARTESIAN_POINT('Ctrl Pts',(39.3662189508584,32.5790975300648,4.17789362839161));
#6400=CARTESIAN_POINT('Ctrl Pts',(38.4998738005519,32.1915847858392,4.2308218681335));
#6401=CARTESIAN_POINT('Ctrl Pts',(37.9946062216704,31.5288056829042,4.28375010787539));
#6402=CARTESIAN_POINT('Ctrl Pts',(37.6647295999779,31.0960937090058,4.31830563775294));
#6403=CARTESIAN_POINT('Ctrl Pts',(37.4887608118784,30.5460505789162,4.35286116763048));
#6404=CARTESIAN_POINT('Ctrl Pts',(37.4850671861185,29.9981671622093,4.38741669750803));
#6405=CARTESIAN_POINT('Origin',(40.,30.,5.));
#6406=CARTESIAN_POINT('',(37.4785970161092,29.9992487947885,5.38741669750803));
#6407=CARTESIAN_POINT('',(37.4815746018733,30.0022201830298,5.11258330249198));
#6408=CARTESIAN_POINT('',(37.4825,30.,5.));
#6409=CARTESIAN_POINT('Ctrl Pts',(37.4815746018733,30.0022201830298,5.11258330249198));
#6410=CARTESIAN_POINT('Ctrl Pts',(37.4800512156624,30.1679668107362,5.10209254006861));
#6411=CARTESIAN_POINT('Ctrl Pts',(37.4950143152585,30.3334397255082,5.09160177764524));
#6412=CARTESIAN_POINT('Ctrl Pts',(37.5274671055976,30.4954083235571,5.08111101522187));
#6413=CARTESIAN_POINT('Ctrl Pts',(37.6911986818205,31.3125760795527,5.02818277547997));
#6414=CARTESIAN_POINT('Ctrl Pts',(38.3001177231744,32.0405439805073,4.97525453573808));
#6415=CARTESIAN_POINT('Ctrl Pts',(39.0754965679032,32.3460907324736,4.92232629599619));
#6416=CARTESIAN_POINT('Ctrl Pts',(39.8508754126321,32.65163748444,4.8693980562543));
#6417=CARTESIAN_POINT('Ctrl Pts',(40.7927140607359,32.5347630874181,4.8164698165124));
#6418=CARTESIAN_POINT('Ctrl Pts',(41.4698936502493,32.0489658313164,4.7635415767705));
#6419=CARTESIAN_POINT('Ctrl Pts',(42.1470732397627,31.5631685752146,4.71061333702861));
#6420=CARTESIAN_POINT('Ctrl Pts',(42.5595937706857,30.7084484600331,4.65768509728672));
#6421=CARTESIAN_POINT('Ctrl Pts',(42.5186273772392,29.8760465588431,4.60475685754482));
#6422=CARTESIAN_POINT('Ctrl Pts',(42.4776609837926,29.0436446576532,4.55182861780293));
#6423=CARTESIAN_POINT('Ctrl Pts',(41.9832076659765,28.2335609704548,4.49890037806103));
#6424=CARTESIAN_POINT('Ctrl Pts',(41.2615993460398,27.8166046141265,4.44597213831914));
#6425=CARTESIAN_POINT('Ctrl Pts',(40.5399910261032,27.3996482577982,4.39304389857724));
#6426=CARTESIAN_POINT('Ctrl Pts',(39.591227704046,27.3758192323399,4.34011565883535));
#6427=CARTESIAN_POINT('Ctrl Pts',(38.8495979541372,27.7560250772875,4.28718741909346));
#6428=CARTESIAN_POINT('Ctrl Pts',(38.1079682042285,28.136230922235,4.23425917935156));
#6429=CARTESIAN_POINT('Ctrl Pts',(37.5734720264681,28.9204716375883,4.18133093960966));
#6430=CARTESIAN_POINT('Ctrl Pts',(37.4907706315128,29.7497675135028,4.12840269986777));
#6431=CARTESIAN_POINT('Ctrl Pts',(37.48253126039,29.8323885683951,4.12312956740917));
#6432=CARTESIAN_POINT('Ctrl Pts',(37.478776282325,29.9154568286489,4.11785643495058));
#6433=CARTESIAN_POINT('Ctrl Pts',(37.4793386265487,29.9985765177349,4.11258330249198));
#6434=CARTESIAN_POINT('Ctrl Pts',(37.4850671861185,29.9981671622093,4.38741669750803));
#6435=CARTESIAN_POINT('Ctrl Pts',(37.4831033350453,29.7068649280859,4.40578940737238));
#6436=CARTESIAN_POINT('Ctrl Pts',(37.5298400476381,29.4161732245676,4.42416211723673));
#6437=CARTESIAN_POINT('Ctrl Pts',(37.6280379842563,29.1440518601549,4.44253482710108));
#6438=CARTESIAN_POINT('Ctrl Pts',(37.9109273331798,28.3601226019852,4.49546306684297));
#6439=CARTESIAN_POINT('Ctrl Pts',(38.620896038483,27.7303095472902,4.54839130658487));
#6440=CARTESIAN_POINT('Ctrl Pts',(39.4329617893699,27.5429044198622,4.60131954632676));
#6441=CARTESIAN_POINT('Ctrl Pts',(40.2450275402567,27.3554992924343,4.65424778606866));
#6442=CARTESIAN_POINT('Ctrl Pts',(41.1591903367271,27.6105020922735,4.70717602581055));
#6443=CARTESIAN_POINT('Ctrl Pts',(41.7569997093075,28.1911873939695,4.76010426555245));
#6444=CARTESIAN_POINT('Ctrl Pts',(42.354809081888,28.7718726956655,4.81303250529434));
#6445=CARTESIAN_POINT('Ctrl Pts',(42.6362650305784,29.6782404992184,4.86596074503623));
#6446=CARTESIAN_POINT('Ctrl Pts',(42.4725334195783,30.4954084287838,4.91888898477813));
#6447=CARTESIAN_POINT('Ctrl Pts',(42.3088018085782,31.3125763583491,4.97181722452002));
#6448=CARTESIAN_POINT('Ctrl Pts',(41.6998826378874,32.040544413927,5.02474546426192));
#6449=CARTESIAN_POINT('Ctrl Pts',(40.924503628465,32.3460912307927,5.07767370400381));
#6450=CARTESIAN_POINT('Ctrl Pts',(40.1491246190426,32.6516380476584,5.13060194374571));
#6451=CARTESIAN_POINT('Ctrl Pts',(39.2072857708885,32.5347636258119,5.1835301834876));
#6452=CARTESIAN_POINT('Ctrl Pts',(38.5301060375394,32.0489662665249,5.2364584232295));
#6453=CARTESIAN_POINT('Ctrl Pts',(37.886304263532,31.5871136942834,5.28677784798901));
#6454=CARTESIAN_POINT('Ctrl Pts',(37.4817146699033,30.7918100700275,5.33709727274852));
#6455=CARTESIAN_POINT('Ctrl Pts',(37.4785970161092,29.9992487947885,5.38741669750803));
#6456=CARTESIAN_POINT('Origin',(40.,30.,5.));
#6457=CARTESIAN_POINT('',(37.4828502770433,30.0023011685704,6.38741669750802));
#6458=CARTESIAN_POINT('',(37.486585582131,30.0000546151574,6.11258330249198));
#6459=CARTESIAN_POINT('',(37.4825,30.,5.));
#6460=CARTESIAN_POINT('Ctrl Pts',(37.486585582131,30.0000546151574,6.11258330249198));
#6461=CARTESIAN_POINT('Ctrl Pts',(37.4865049295332,30.4169561491143,6.08632864518665));
#6462=CARTESIAN_POINT('Ctrl Pts',(37.584530250577,30.8338220003565,6.06007398788131));
#6463=CARTESIAN_POINT('Ctrl Pts',(37.7808708979026,31.1976286357266,6.03381933057598));
#6464=CARTESIAN_POINT('Ctrl Pts',(38.1766850474407,31.9310468857773,5.98089109083408));
#6465=CARTESIAN_POINT('Ctrl Pts',(38.9720604978366,32.4488282649741,5.92796285109219));
#6466=CARTESIAN_POINT('Ctrl Pts',(39.8029207061802,32.5139626236142,5.87503461135029));
#6467=CARTESIAN_POINT('Ctrl Pts',(40.6337809145239,32.5790969822544,5.8221063716084));
#6468=CARTESIAN_POINT('Ctrl Pts',(41.5001258808154,32.1915843203379,5.7691781318665));
#6469=CARTESIAN_POINT('Ctrl Pts',(42.005393352376,31.5288053581798,5.71624989212461));
#6470=CARTESIAN_POINT('Ctrl Pts',(42.5106608239366,30.8660263960216,5.66332165238271));
#6471=CARTESIAN_POINT('Ctrl Pts',(42.6548508007663,29.9279811336217,5.61039341264082));
#6472=CARTESIAN_POINT('Ctrl Pts',(42.3719615119296,29.1440520419617,5.55746517289892));
#6473=CARTESIAN_POINT('Ctrl Pts',(42.0890722230929,28.3601229503016,5.50453693315703));
#6474=CARTESIAN_POINT('Ctrl Pts',(41.3791036685898,27.7303100293814,5.45160869341513));
#6475=CARTESIAN_POINT('Ctrl Pts',(40.567038090189,27.5429049417591,5.39868045367324));
#6476=CARTESIAN_POINT('Ctrl Pts',(39.7549725117881,27.3554998541367,5.34575221393134));
#6477=CARTESIAN_POINT('Ctrl Pts',(38.8408099094895,27.6105025998123,5.29282397418945));
#6478=CARTESIAN_POINT('Ctrl Pts',(38.2430006638861,28.1911877781685,5.23989573444756));
#6479=CARTESIAN_POINT('Ctrl Pts',(37.7636815626878,28.6567769269077,5.19745825712903));
#6480=CARTESIAN_POINT('Ctrl Pts',(37.4877370393744,29.3317380512216,5.15502077981051));
#6481=CARTESIAN_POINT('Ctrl Pts',(37.4815746018733,30.0022201830298,5.11258330249198));
#6482=CARTESIAN_POINT('Ctrl Pts',(37.4785970161092,29.9992487947885,5.38741669750803));
#6483=CARTESIAN_POINT('Ctrl Pts',(37.4784353810753,29.9581583860809,5.39002551249041));
#6484=CARTESIAN_POINT('Ctrl Pts',(37.4793528677292,29.9170753485691,5.39263432747279));
#6485=CARTESIAN_POINT('Ctrl Pts',(37.4813720877943,29.8760465325149,5.39524314245518));
#6486=CARTESIAN_POINT('Ctrl Pts',(37.5223384899423,29.0436444545195,5.44817138219707));
#6487=CARTESIAN_POINT('Ctrl Pts',(38.0167919127822,28.2335605952563,5.50109962193897));
#6488=CARTESIAN_POINT('Ctrl Pts',(38.7384003859914,27.8166041503647,5.55402786168086));
#6489=CARTESIAN_POINT('Ctrl Pts',(39.4600088592005,27.3996477054731,5.60695610142276));
#6490=CARTESIAN_POINT('Ctrl Pts',(40.4087723827788,27.3758186749531,5.65988434116465));
#6491=CARTESIAN_POINT('Ctrl Pts',(41.1504022902127,27.756024600658,5.71281258090654));
#6492=CARTESIAN_POINT('Ctrl Pts',(41.8920321976466,28.1362305263629,5.76574082064844));
#6493=CARTESIAN_POINT('Ctrl Pts',(42.4265284889361,28.9204714082927,5.81866906039033));
#6494=CARTESIAN_POINT('Ctrl Pts',(42.5092299014576,29.7497674603527,5.87159730013223));
#6495=CARTESIAN_POINT('Ctrl Pts',(42.591931313979,30.5790635124127,5.92452553987413));
#6496=CARTESIAN_POINT('Ctrl Pts',(42.2228378477325,31.4534147346028,5.97745377961602));
#6497=CARTESIAN_POINT('Ctrl Pts',(41.5708989883459,31.9725940765548,6.03038201935791));
#6498=CARTESIAN_POINT('Ctrl Pts',(40.9189601289592,32.4917734185068,6.08331025909981));
#6499=CARTESIAN_POINT('Ctrl Pts',(39.9841758764325,32.6557808802207,6.1362384988417));
#6500=CARTESIAN_POINT('Ctrl Pts',(39.1944360013915,32.3895434011234,6.1891667385836));
#6501=CARTESIAN_POINT('Ctrl Pts',(38.4046961263506,32.123305922026,6.24209497832549));
#6502=CARTESIAN_POINT('Ctrl Pts',(37.7600006287953,31.4268235021173,6.29502321806738));
#6503=CARTESIAN_POINT('Ctrl Pts',(37.5554535478708,30.6189052156672,6.34795145780928));
#6504=CARTESIAN_POINT('Ctrl Pts',(37.5046142755673,30.418100698789,6.36110653770886));
#6505=CARTESIAN_POINT('Ctrl Pts',(37.4809651294343,30.2104122419562,6.37426161760844));
#6506=CARTESIAN_POINT('Ctrl Pts',(37.4828502770433,30.0023011685704,6.38741669750802));
#6507=CARTESIAN_POINT('Origin',(40.,30.,5.));
#6508=CARTESIAN_POINT('',(37.4864394344908,29.9993677916106,7.38741669750803));
#6509=CARTESIAN_POINT('',(37.4817751445882,29.9977519262233,7.11258330249198));
#6510=CARTESIAN_POINT('',(37.4825,30.,5.));
#6511=CARTESIAN_POINT('Ctrl Pts',(37.4817751445882,29.9977519262233,7.11258330249198));
#6512=CARTESIAN_POINT('Ctrl Pts',(37.4879010544836,30.6617513350285,7.07056475030468));
#6513=CARTESIAN_POINT('Ctrl Pts',(37.7578397626965,31.3301554940639,7.02854619811738));
#6514=CARTESIAN_POINT('Ctrl Pts',(38.22877221091,31.7948817330614,6.98652764593008));
#6515=CARTESIAN_POINT('Ctrl Pts',(38.8219774553499,32.3802693895033,6.93359940618818));
#6516=CARTESIAN_POINT('Ctrl Pts',(39.7340979334441,32.6424828443064,6.88067116644629));
#6517=CARTESIAN_POINT('Ctrl Pts',(40.5476180320737,32.4614960518533,6.82774292670439));
#6518=CARTESIAN_POINT('Ctrl Pts',(41.3611381307034,32.2805092594003,6.7748146869625));
#6519=CARTESIAN_POINT('Ctrl Pts',(42.0760578498686,31.6563222196911,6.7218864472206));
#6520=CARTESIAN_POINT('Ctrl Pts',(42.3651285920733,30.8746513958526,6.66895820747871));
#6521=CARTESIAN_POINT('Ctrl Pts',(42.654199334278,30.0929805720141,6.61602996773681));
#6522=CARTESIAN_POINT('Ctrl Pts',(42.5174210995221,29.1538259640462,6.56310172799492));
#6523=CARTESIAN_POINT('Ctrl Pts',(42.0174029955306,28.487077836095,6.51017348825303));
#6524=CARTESIAN_POINT('Ctrl Pts',(41.517384891539,27.8203297081438,6.45724524851113));
#6525=CARTESIAN_POINT('Ctrl Pts',(40.6541269183117,27.4259880602093,6.40431700876923));
#6526=CARTESIAN_POINT('Ctrl Pts',(39.8227782826846,27.4845595248407,6.35138876902734));
#6527=CARTESIAN_POINT('Ctrl Pts',(38.9914296470575,27.5431309894721,6.29846052928544));
#6528=CARTESIAN_POINT('Ctrl Pts',(38.1919903490306,28.0546155666694,6.24553228954355));
#6529=CARTESIAN_POINT('Ctrl Pts',(37.7903971243573,28.7848854157204,6.19260404980166));
#6530=CARTESIAN_POINT('Ctrl Pts',(37.5880112139904,29.1529103701602,6.1659304673651));
#6531=CARTESIAN_POINT('Ctrl Pts',(37.4866675216396,29.5765009079199,6.13925688492854));
#6532=CARTESIAN_POINT('Ctrl Pts',(37.486585582131,30.0000546151574,6.11258330249198));
#6533=CARTESIAN_POINT('Ctrl Pts',(37.4828502770433,30.0023011685704,6.38741669750802));
#6534=CARTESIAN_POINT('Ctrl Pts',(37.488549845404,29.3730967053584,6.42718985735034));
#6535=CARTESIAN_POINT('Ctrl Pts',(37.7276581251219,28.7400291086663,6.46696301719265));
#6536=CARTESIAN_POINT('Ctrl Pts',(38.1544129894185,28.2816695282955,6.50673617703496));
#6537=CARTESIAN_POINT('Ctrl Pts',(38.7223181761841,27.6717062803654,6.55966441677686));
#6538=CARTESIAN_POINT('Ctrl Pts',(39.622527214009,27.3711339374966,6.61259265651875));
#6539=CARTESIAN_POINT('Ctrl Pts',(40.4429768514351,27.5175370039119,6.66552089626065));
#6540=CARTESIAN_POINT('Ctrl Pts',(41.2634264888611,27.6639400703271,6.71844913600254));
#6541=CARTESIAN_POINT('Ctrl Pts',(42.0041167258884,28.2573185460263,6.77137737574444));
#6542=CARTESIAN_POINT('Ctrl Pts',(42.3260027238261,29.026058341056,6.82430561548633));
#6543=CARTESIAN_POINT('Ctrl Pts',(42.6478887217638,29.7947981360857,6.87723385522822));
#6544=CARTESIAN_POINT('Ctrl Pts',(42.5509704806119,30.7388992504459,6.93016209497012));
#6545=CARTESIAN_POINT('Ctrl Pts',(42.0796115257342,31.4262071844781,6.98309033471202));
#6546=CARTESIAN_POINT('Ctrl Pts',(41.6082525708565,32.1135151185102,7.03601857445391));
#6547=CARTESIAN_POINT('Ctrl Pts',(40.7624529022529,32.5440298722143,7.0889468141958));
#6548=CARTESIAN_POINT('Ctrl Pts',(39.9293703303048,32.5206868978311,7.1418750539377));
#6549=CARTESIAN_POINT('Ctrl Pts',(39.0962877583566,32.4973439234479,7.19480329367959));
#6550=CARTESIAN_POINT('Ctrl Pts',(38.2759222830639,32.0201432209773,7.24773153342149));
#6551=CARTESIAN_POINT('Ctrl Pts',(37.8437894287741,31.3075194208077,7.30065977316339));
#6552=CARTESIAN_POINT('Ctrl Pts',(37.6076803275377,30.9181554478826,7.32957874794493));
#6553=CARTESIAN_POINT('Ctrl Pts',(37.4874710852924,30.4585101478601,7.35849772272648));
#6554=CARTESIAN_POINT('Ctrl Pts',(37.4864394344908,29.9993677916106,7.38741669750803));
#6555=CARTESIAN_POINT('Origin',(40.,30.,5.));
#6556=CARTESIAN_POINT('',(37.4805317771007,29.9980220368919,8.38741669750803));
#6557=CARTESIAN_POINT('',(37.4791973108607,30.0013273487219,8.11258330249198));
#6558=CARTESIAN_POINT('',(37.4825,30.,5.));
#6559=CARTESIAN_POINT('Ctrl Pts',(37.4791973108607,30.0013273487219,8.11258330249198));
#6560=CARTESIAN_POINT('Ctrl Pts',(37.4787079525275,30.0778322873578,8.10772909516461));
#6561=CARTESIAN_POINT('Ctrl Pts',(37.4818888734735,30.1542959784042,8.10287488783723));
#6562=CARTESIAN_POINT('Ctrl Pts',(37.4888728396115,30.2304107157375,8.09802068050986));
#6563=CARTESIAN_POINT('Ctrl Pts',(37.5650230757208,31.0603338718311,8.04509244076797));
#6564=CARTESIAN_POINT('Ctrl Pts',(38.0933099956412,31.8487705962177,7.99216420102607));
#6565=CARTESIAN_POINT('Ctrl Pts',(38.8319143740251,32.2348208014644,7.93923596128418));
#6566=CARTESIAN_POINT('Ctrl Pts',(39.570518752409,32.620871006711,7.88630772154228));
#6567=CARTESIAN_POINT('Ctrl Pts',(40.5194405892562,32.6045346928177,7.83337948180038));
#6568=CARTESIAN_POINT('Ctrl Pts',(41.2443188772582,32.1932895167892,7.78045124205849));
#6569=CARTESIAN_POINT('Ctrl Pts',(41.9691971652602,31.7820443407606,7.7275230023166));
#6570=CARTESIAN_POINT('Ctrl Pts',(42.4700319044171,30.9758903025967,7.67459476257471));
#6571=CARTESIAN_POINT('Ctrl Pts',(42.5175700665678,30.1438378327645,7.62166652283281));
#6572=CARTESIAN_POINT('Ctrl Pts',(42.5651082287186,29.3117853629323,7.56873828309092));
#6573=CARTESIAN_POINT('Ctrl Pts',(42.1593498138633,28.4538344614319,7.51581004334902));
#6574=CARTESIAN_POINT('Ctrl Pts',(41.4860274165556,27.962705028035,7.46288180360712));
#6575=CARTESIAN_POINT('Ctrl Pts',(40.8127050192479,27.4715755946381,7.40995356386523));
#6576=CARTESIAN_POINT('Ctrl Pts',(39.8718186394878,27.3472676293449,7.35702532412334));
#6577=CARTESIAN_POINT('Ctrl Pts',(39.0940512304695,27.6466820960993,7.30409708438144));
#6578=CARTESIAN_POINT('Ctrl Pts',(38.3162838214513,27.9460965628537,7.25116884463955));
#6579=CARTESIAN_POINT('Ctrl Pts',(37.7016353831749,28.6692334616558,7.19824060489765));
#6580=CARTESIAN_POINT('Ctrl Pts',(37.5314561694296,29.4850828400972,7.14531236515576));
#6581=CARTESIAN_POINT('Ctrl Pts',(37.4963784479845,29.6532475448712,7.13440267760117));
#6582=CARTESIAN_POINT('Ctrl Pts',(37.480184614704,29.8253512672427,7.12349299004657));
#6583=CARTESIAN_POINT('Ctrl Pts',(37.4817751445882,29.9977519262233,7.11258330249198));
#6584=CARTESIAN_POINT('Ctrl Pts',(37.4864394344908,29.9993677916106,7.38741669750803));
#6585=CARTESIAN_POINT('Ctrl Pts',(37.4855829318786,29.6181761840593,7.41142596246837));
#6586=CARTESIAN_POINT('Ctrl Pts',(37.5668724532984,29.2373312426116,7.43543522742871));
#6587=CARTESIAN_POINT('Ctrl Pts',(37.7321836902776,28.8973394634674,7.45944449238906));
#6588=CARTESIAN_POINT('Ctrl Pts',(38.0966110393577,28.1478302041652,7.51237273213095));
#6589=CARTESIAN_POINT('Ctrl Pts',(38.8693659708049,27.5968585834295,7.56530097187285));
#6590=CARTESIAN_POINT('Ctrl Pts',(39.6967263130212,27.4966271115958,7.61822921161475));
#6591=CARTESIAN_POINT('Ctrl Pts',(40.5240866552375,27.396395639762,7.67115745135664));
#6592=CARTESIAN_POINT('Ctrl Pts',(41.406052408223,27.7469043168303,7.72408569109854));
#6593=CARTESIAN_POINT('Ctrl Pts',(41.9389110020029,28.3877110869611,7.77701393084043));
#6594=CARTESIAN_POINT('Ctrl Pts',(42.4717695957828,29.0285178570919,7.82994217058232));
#6595=CARTESIAN_POINT('Ctrl Pts',(42.6555210303571,29.9596227202852,7.88287041032422));
#6596=CARTESIAN_POINT('Ctrl Pts',(42.4060546666335,30.7548193248618,7.93579865006612));
#6597=CARTESIAN_POINT('Ctrl Pts',(42.1565883029099,31.5500159294385,7.98872688980801));
#6598=CARTESIAN_POINT('Ctrl Pts',(41.4739041408884,32.2093042753983,8.04165512954991));
#6599=CARTESIAN_POINT('Ctrl Pts',(40.670495092448,32.4309021481149,8.0945833692918));
#6600=CARTESIAN_POINT('Ctrl Pts',(39.8670860440077,32.6525000208315,8.1475116090337));
#6601=CARTESIAN_POINT('Ctrl Pts',(38.9429521091486,32.4364074203047,8.20043984877559));
#6602=CARTESIAN_POINT('Ctrl Pts',(38.3211082124662,31.8815357928507,8.25336808851748));
#6603=CARTESIAN_POINT('Ctrl Pts',(37.7961376122345,31.413104257428,8.298050958181));
#6604=CARTESIAN_POINT('Ctrl Pts',(37.4866093473163,30.7032246572373,8.34273382784451));
#6605=CARTESIAN_POINT('Ctrl Pts',(37.4805317771007,29.9980220368919,8.38741669750803));
#6606=CARTESIAN_POINT('Origin',(40.,30.,5.));
#6607=CARTESIAN_POINT('',(37.480218046669,30.0018167092234,9.38741669750803));
#6608=CARTESIAN_POINT('',(37.4857777211518,30.0014129073083,9.11258330249198));
#6609=CARTESIAN_POINT('',(37.4825,30.,5.));
#6610=CARTESIAN_POINT('',(41.9134659966651,31.6359872033749,10.));
#6611=CARTESIAN_POINT('Ctrl Pts',(37.480218046669,30.0018167092234,9.38741669750803));
#6612=CARTESIAN_POINT('Ctrl Pts',(37.4861413026091,29.2855374632777,9.43282641244634));
#6613=CARTESIAN_POINT('Ctrl Pts',(37.8070286664086,28.564752250932,9.47823612738464));
#6614=CARTESIAN_POINT('Ctrl Pts',(38.3470250748122,28.0958621231864,9.52364584232295));
#6615=CARTESIAN_POINT('Ctrl Pts',(38.9764291440202,27.5493374615002,9.57657408206485));
#6616=CARTESIAN_POINT('Ctrl Pts',(39.9035049870189,27.3450262249946,9.62950232180674));
#6617=CARTESIAN_POINT('Ctrl Pts',(40.7037784842569,27.5780866607079,9.68243056154864));
#6618=CARTESIAN_POINT('Ctrl Pts',(41.5040519814949,27.8111470964211,9.73535880129053));
#6619=CARTESIAN_POINT('Ctrl Pts',(42.1775231329722,28.4815792043531,9.78828704103243));
#6620=CARTESIAN_POINT('Ctrl Pts',(42.415891769617,29.278704654386,9.84121528077432));
#6621=CARTESIAN_POINT('Ctrl Pts',(42.6542604062617,30.075830104419,9.89414352051621));
#6622=CARTESIAN_POINT('Ctrl Pts',(42.4575265280738,30.9996488965529,9.94707176025811));
#6623=CARTESIAN_POINT('Ctrl Pts',(41.9134659966651,31.6359872033749,10.));
#6624=CARTESIAN_POINT('',(38.0828938975876,31.638757370194,10.));
#6625=CARTESIAN_POINT('Origin',(40.,30.,10.));
#6626=CARTESIAN_POINT('Ctrl Pts',(38.082890958175,31.6387596071244,10.));
#6627=CARTESIAN_POINT('Ctrl Pts',(38.6136992476573,32.2578638410584,9.94821753066412));
#6628=CARTESIAN_POINT('Ctrl Pts',(39.473300026191,32.5973559811872,9.89643506132825));
#6629=CARTESIAN_POINT('Ctrl Pts',(40.2836371055782,32.5055162560996,9.84465259199238));
#6630=CARTESIAN_POINT('Ctrl Pts',(41.1119041959588,32.4116444294059,9.79172435225048));
#6631=CARTESIAN_POINT('Ctrl Pts',(41.8887033912065,31.867141740819,9.73879611250859));
#6632=CARTESIAN_POINT('Ctrl Pts',(42.2589673171139,31.1206210491648,9.68586787276669));
#6633=CARTESIAN_POINT('Ctrl Pts',(42.6292312430212,30.3741003575106,9.6329396330248));
#6634=CARTESIAN_POINT('Ctrl Pts',(42.5929598995882,29.4255616627892,9.58001139328291));
#6635=CARTESIAN_POINT('Ctrl Pts',(42.1665030878871,28.7095042477308,9.52708315354101));
#6636=CARTESIAN_POINT('Ctrl Pts',(41.740046276186,27.9934468326725,9.47415491379912));
#6637=CARTESIAN_POINT('Ctrl Pts',(40.9234039962168,27.5098706972773,9.42122667405722));
#6638=CARTESIAN_POINT('Ctrl Pts',(40.0905142414943,27.4799719042595,9.36829843431532));
#6639=CARTESIAN_POINT('Ctrl Pts',(39.2576244867719,27.4500731112417,9.31537019457343));
#6640=CARTESIAN_POINT('Ctrl Pts',(38.408487257296,27.8738516606013,9.26244195483154));
#6641=CARTESIAN_POINT('Ctrl Pts',(37.9317246371012,28.557405001666,9.20951371508965));
#6642=CARTESIAN_POINT('Ctrl Pts',(37.640684052642,28.9746813473057,9.17720357755709));
#6643=CARTESIAN_POINT('Ctrl Pts',(37.4884093731962,29.4887631226718,9.14489344002454));
#6644=CARTESIAN_POINT('Ctrl Pts',(37.4857777211518,30.0014129073083,9.11258330249198));
#6645=CARTESIAN_POINT('Origin',(-40.,30.,5.));
#6646=CARTESIAN_POINT('',(-42.5134503279812,30.0006057610914,0.387416697508013));
#6647=CARTESIAN_POINT('',(-42.5156179788862,29.9964982081097,0.112583302491982));
#6648=CARTESIAN_POINT('',(-42.5175,30.,5.));
#6649=CARTESIAN_POINT('',(-41.9134659966651,31.635987203375,0.));
#6650=CARTESIAN_POINT('Ctrl Pts',(-42.5156179788862,29.9964982081097,0.112583302491982));
#6651=CARTESIAN_POINT('Ctrl Pts',(-42.510368759274,30.5890972399227,0.0750555349946548));
#6652=CARTESIAN_POINT('Ctrl Pts',(-42.2992218280841,31.1848035603044,0.0375277674973275));
#6653=CARTESIAN_POINT('Ctrl Pts',(-41.9134659966651,31.635987203375,0.));
#6654=CARTESIAN_POINT('',(-38.0828938060045,31.6387572824072,1.01111975331451E-14));
#6655=CARTESIAN_POINT('Origin',(-40.,30.,0.));
#6656=CARTESIAN_POINT('Ctrl Pts',(-38.0828908636836,31.6387595214235,6.73072708679001E-15));
#6657=CARTESIAN_POINT('Ctrl Pts',(-38.6136991238565,32.2578636190535,0.0517824693358767));
#6658=CARTESIAN_POINT('Ctrl Pts',(-39.4732999763485,32.5973561213315,0.103564938671746));
#6659=CARTESIAN_POINT('Ctrl Pts',(-40.2836371098419,32.5055164690084,0.155347408007616));
#6660=CARTESIAN_POINT('Ctrl Pts',(-41.111904255526,32.4116447166893,0.20827564774951));
#6661=CARTESIAN_POINT('Ctrl Pts',(-41.888703485337,31.8671418001444,0.261203887491404));
#6662=CARTESIAN_POINT('Ctrl Pts',(-42.2589674214213,31.120621033114,0.314132127233298));
#6663=CARTESIAN_POINT('Ctrl Pts',(-42.4298568720969,30.7760762061322,0.33856031732487));
#6664=CARTESIAN_POINT('Ctrl Pts',(-42.514148706906,30.3884987950563,0.362988507416442));
#6665=CARTESIAN_POINT('Ctrl Pts',(-42.5134503279812,30.0006057610914,0.387416697508013));
#6666=CARTESIAN_POINT('Origin',(-40.,30.,5.));
#6667=CARTESIAN_POINT('',(-42.5173482652661,29.997696535754,1.38741669750801));
#6668=CARTESIAN_POINT('',(-42.5216690254717,30.000121302647,1.11258330249199));
#6669=CARTESIAN_POINT('',(-42.5175,30.,5.));
#6670=CARTESIAN_POINT('Ctrl Pts',(-42.5216690254717,30.000121302647,1.11258330249199));
#6671=CARTESIAN_POINT('Ctrl Pts',(-42.5216725769877,30.0058437075332,1.11221987985459));
#6672=CARTESIAN_POINT('Ctrl Pts',(-42.5216547894118,30.0115660877676,1.11185645721719));
#6673=CARTESIAN_POINT('Ctrl Pts',(-42.5216155963134,30.0172883193759,1.11149303457979));
#6674=CARTESIAN_POINT('Ctrl Pts',(-42.515907581752,30.8506641613213,1.0585647948379));
#6675=CARTESIAN_POINT('Ctrl Pts',(-42.0561776880642,31.6808875687602,1.005636555096));
#6676=CARTESIAN_POINT('Ctrl Pts',(-41.3528556457226,32.1280312515289,0.952708315354107));
#6677=CARTESIAN_POINT('Ctrl Pts',(-40.6495336033811,32.5751749342975,0.899780075612213));
#6678=CARTESIAN_POINT('Ctrl Pts',(-39.7026194123857,32.6392388923959,0.846851835870317));
#6679=CARTESIAN_POINT('Ctrl Pts',(-38.9455708556586,32.2906974313558,0.793923596128423));
#6680=CARTESIAN_POINT('Ctrl Pts',(-38.1885222989315,31.9421559703156,0.74099535638653));
#6681=CARTESIAN_POINT('Ctrl Pts',(-37.6213393764727,31.181009090137,0.688067116644636));
#6682=CARTESIAN_POINT('Ctrl Pts',(-37.5036142405306,30.3560669733062,0.635138876902743));
#6683=CARTESIAN_POINT('Ctrl Pts',(-37.3858891045884,29.5311248564754,0.582210637160847));
#6684=CARTESIAN_POINT('Ctrl Pts',(-37.717621755163,28.6423875029925,0.529282397418951));
#6685=CARTESIAN_POINT('Ctrl Pts',(-38.3470255141114,28.0958627356919,0.476354157677056));
#6686=CARTESIAN_POINT('Ctrl Pts',(-38.9764292730598,27.5493379683914,0.423425917935162));
#6687=CARTESIAN_POINT('Ctrl Pts',(-39.9035041403819,27.3450257872733,0.370497678193267));
#6688=CARTESIAN_POINT('Ctrl Pts',(-40.7037780644453,27.5780866271583,0.317569438451373));
#6689=CARTESIAN_POINT('Ctrl Pts',(-41.5040519885087,27.8111474670432,0.264641198709479));
#6690=CARTESIAN_POINT('Ctrl Pts',(-42.1775249693132,28.4815813279313,0.211712958967585));
#6691=CARTESIAN_POINT('Ctrl Pts',(-42.4158936042045,29.2787066853087,0.158784719225691));
#6692=CARTESIAN_POINT('Ctrl Pts',(-42.485251466161,29.5106453819591,0.143384246981121));
#6693=CARTESIAN_POINT('Ctrl Pts',(-42.5177721294348,29.753310148968,0.127983774736552));
#6694=CARTESIAN_POINT('Ctrl Pts',(-42.5156179788862,29.9964982081097,0.112583302491982));
#6695=CARTESIAN_POINT('Ctrl Pts',(-42.5134503279812,30.0006057610914,0.387416697508013));
#6696=CARTESIAN_POINT('Ctrl Pts',(-42.5126355384304,29.5480560353207,0.415916747158336));
#6697=CARTESIAN_POINT('Ctrl Pts',(-42.3961356098422,29.0950766968195,0.444416796808659));
#6698=CARTESIAN_POINT('Ctrl Pts',(-42.1665031701499,28.7095042291822,0.472916846458981));
#6699=CARTESIAN_POINT('Ctrl Pts',(-41.7400463404364,27.9934468097964,0.525845086200876));
#6700=CARTESIAN_POINT('Ctrl Pts',(-40.9234040386519,27.5098705885405,0.578773325942772));
#6701=CARTESIAN_POINT('Ctrl Pts',(-40.0905142507848,27.4799717796994,0.631701565684667));
#6702=CARTESIAN_POINT('Ctrl Pts',(-39.2576244629178,27.4500729708583,0.684629805426561));
#6703=CARTESIAN_POINT('Ctrl Pts',(-38.4084871889682,27.8738515744319,0.737558045168454));
#6704=CARTESIAN_POINT('Ctrl Pts',(-37.9317245473703,28.5574049522032,0.790486284910349));
#6705=CARTESIAN_POINT('Ctrl Pts',(-37.4549619057724,29.2409583299746,0.843414524652243));
#6706=CARTESIAN_POINT('Ctrl Pts',(-37.3505738965262,30.1842864819436,0.896342764394139));
#6707=CARTESIAN_POINT('Ctrl Pts',(-37.6663750453751,30.9555494190257,0.949271004136033));
#6708=CARTESIAN_POINT('Ctrl Pts',(-37.982176194224,31.7268123561078,1.00219924387793));
#6709=CARTESIAN_POINT('Ctrl Pts',(-38.718166501168,32.326010078303,1.05512748361982));
#6710=CARTESIAN_POINT('Ctrl Pts',(-39.5374365691663,32.4788844674016,1.10805572336172));
#6711=CARTESIAN_POINT('Ctrl Pts',(-40.3567066371647,32.6317588565003,1.16098396310361));
#6712=CARTESIAN_POINT('Ctrl Pts',(-41.2592564662174,32.3383099125024,1.2139122028455));
#6713=CARTESIAN_POINT('Ctrl Pts',(-41.831959295633,31.7328516054719,1.2668404425874));
#6714=CARTESIAN_POINT('Ctrl Pts',(-42.2668522922017,31.2730851019424,1.30703252756094));
#6715=CARTESIAN_POINT('Ctrl Pts',(-42.5115416993795,30.6334009370801,1.34722461253448));
#6716=CARTESIAN_POINT('Ctrl Pts',(-42.5173482652661,29.997696535754,1.38741669750801));
#6717=CARTESIAN_POINT('Origin',(-40.,30.,5.));
#6718=CARTESIAN_POINT('',(-42.521313086871,30.0008653513074,2.38741669750802));
#6719=CARTESIAN_POINT('',(-42.515808333435,30.0021290957888,2.11258330249199));
#6720=CARTESIAN_POINT('',(-42.5175,30.,5.));
#6721=CARTESIAN_POINT('Ctrl Pts',(-42.515808333435,30.0021290957888,2.11258330249199));
#6722=CARTESIAN_POINT('Ctrl Pts',(-42.5178586186008,30.2576058506372,2.09645598497262));
#6723=CARTESIAN_POINT('Ctrl Pts',(-42.4820670914407,30.5125215998601,2.08032866745326));
#6724=CARTESIAN_POINT('Ctrl Pts',(-42.4060543110146,30.7548192142433,2.06420134993389));
#6725=CARTESIAN_POINT('Ctrl Pts',(-42.1565879840197,31.5500157004268,2.011273110192));
#6726=CARTESIAN_POINT('Ctrl Pts',(-41.4739039223289,32.2093039453825,1.9583448704501));
#6727=CARTESIAN_POINT('Ctrl Pts',(-40.6704949930077,32.430901786829,1.90541663070821));
#6728=CARTESIAN_POINT('Ctrl Pts',(-39.8670860636866,32.6524996282756,1.85248839096631));
#6729=CARTESIAN_POINT('Ctrl Pts',(-38.9429522667351,32.4364070662131,1.79956015122442));
#6730=CARTESIAN_POINT('Ctrl Pts',(-38.3211084613291,31.8815355180746,1.74663191148252));
#6731=CARTESIAN_POINT('Ctrl Pts',(-37.6992646559231,31.3266639699361,1.69370367174063));
#6732=CARTESIAN_POINT('Ctrl Pts',(-37.3797108420626,30.4330134357218,1.64077543199874));
#6733=CARTESIAN_POINT('Ctrl Pts',(-37.5087196462193,29.6096513927718,1.58784719225684));
#6734=CARTESIAN_POINT('Ctrl Pts',(-37.637728450376,28.7862893498218,1.53491895251495));
#6735=CARTESIAN_POINT('Ctrl Pts',(-38.2152998725499,28.0332157981361,1.48199071277305));
#6736=CARTESIAN_POINT('Ctrl Pts',(-38.9770563481404,27.6951313019726,1.42906247303116));
#6737=CARTESIAN_POINT('Ctrl Pts',(-39.7388128237309,27.3570468058091,1.37613423328926));
#6738=CARTESIAN_POINT('Ctrl Pts',(-40.6847543527379,27.4339513651679,1.32320599354737));
#6739=CARTESIAN_POINT('Ctrl Pts',(-41.3818820495239,27.8906677830732,1.27027775380548));
#6740=CARTESIAN_POINT('Ctrl Pts',(-42.0742230391115,28.344248236398,1.21771293670098));
#6741=CARTESIAN_POINT('Ctrl Pts',(-42.5211553403926,29.1724426297002,1.16514811959648));
#6742=CARTESIAN_POINT('Ctrl Pts',(-42.5216690254717,30.000121302647,1.11258330249199));
#6743=CARTESIAN_POINT('Ctrl Pts',(-42.5173482652661,29.997696535754,1.38741669750801));
#6744=CARTESIAN_POINT('Ctrl Pts',(-42.5191882624162,29.79625315088,1.40015285227637));
#6745=CARTESIAN_POINT('Ctrl Pts',(-42.4970410052288,29.595209391193,1.41288900704473));
#6746=CARTESIAN_POINT('Ctrl Pts',(-42.4493575441589,29.4004167811413,1.42562516181308));
#6747=CARTESIAN_POINT('Ctrl Pts',(-42.2511971334908,28.5909079339042,1.47855340155498));
#6748=CARTESIAN_POINT('Ctrl Pts',(-41.6120204823761,27.8893579094928,1.53148164129687));
#6749=CARTESIAN_POINT('Ctrl Pts',(-40.8244074219312,27.6168929643317,1.58440988103877));
#6750=CARTESIAN_POINT('Ctrl Pts',(-40.0367943614864,27.3444280191707,1.63733812078066));
#6751=CARTESIAN_POINT('Ctrl Pts',(-39.1007448917115,27.50104815326,1.69026636052255));
#6752=CARTESIAN_POINT('Ctrl Pts',(-38.4447269252528,28.0150630321248,1.74319460026445));
#6753=CARTESIAN_POINT('Ctrl Pts',(-37.7887089587941,28.5290779109896,1.79612284000634));
#6754=CARTESIAN_POINT('Ctrl Pts',(-37.4127224956517,29.4004875346298,1.84905107974824));
#6755=CARTESIAN_POINT('Ctrl Pts',(-37.4888727349885,30.2304107252086,1.90197931949013));
#6756=CARTESIAN_POINT('Ctrl Pts',(-37.5650229743253,31.0603339157874,1.95490755923203));
#6757=CARTESIAN_POINT('Ctrl Pts',(-38.0933099161414,31.8487706733048,2.00783579897392));
#6758=CARTESIAN_POINT('Ctrl Pts',(-38.8319143252891,32.2348208947076,2.06076403871582));
#6759=CARTESIAN_POINT('Ctrl Pts',(-39.5705187344369,32.6208711161104,2.11369227845771));
#6760=CARTESIAN_POINT('Ctrl Pts',(-40.5194406109162,32.6045348013986,2.16662051819961));
#6761=CARTESIAN_POINT('Ctrl Pts',(-41.2443189291553,32.1932896081922,2.2195487579415));
#6762=CARTESIAN_POINT('Ctrl Pts',(-41.9691972473944,31.7820444149859,2.27247699768339));
#6763=CARTESIAN_POINT('Ctrl Pts',(-42.4700320073933,30.975890343285,2.32540523742529));
#6764=CARTESIAN_POINT('Ctrl Pts',(-42.5175701715172,30.1438378387809,2.37833347716718));
#6765=CARTESIAN_POINT('Ctrl Pts',(-42.5202895743756,30.0962405871662,2.3813612172808));
#6766=CARTESIAN_POINT('Ctrl Pts',(-42.5215256234437,30.0485585863193,2.38438895739441));
#6767=CARTESIAN_POINT('Ctrl Pts',(-42.521313086871,30.0008653513074,2.38741669750802));
#6768=CARTESIAN_POINT('Origin',(-40.,30.,5.));
#6769=CARTESIAN_POINT('',(-42.5147865997281,30.0017637212727,3.38741669750802));
#6770=CARTESIAN_POINT('',(-42.5141171500829,29.9986698323151,3.11258330249199));
#6771=CARTESIAN_POINT('',(-42.5175,30.,5.));
#6772=CARTESIAN_POINT('Ctrl Pts',(-42.5141171500829,29.9986698323151,3.11258330249199));
#6773=CARTESIAN_POINT('Ctrl Pts',(-42.5116924647915,30.5047215402099,3.08069209009066));
#6774=CARTESIAN_POINT('Ctrl Pts',(-42.3636222943308,31.0120787091108,3.04880087768933));
#6775=CARTESIAN_POINT('Ctrl Pts',(-42.0796112182407,31.4262069736182,3.01690966528799));
#6776=CARTESIAN_POINT('Ctrl Pts',(-41.608252333057,32.1135148060047,2.9639814255461));
#6777=CARTESIAN_POINT('Ctrl Pts',(-40.7624527895073,32.544029495972,2.9110531858042));
#6778=CARTESIAN_POINT('Ctrl Pts',(-39.9293703407444,32.5206865250762,2.85812494606231));
#6779=CARTESIAN_POINT('Ctrl Pts',(-39.0962878919816,32.4973435541803,2.80519670632041));
#6780=CARTESIAN_POINT('Ctrl Pts',(-38.2759225380058,32.0201429224212,2.75226846657852));
#6781=CARTESIAN_POINT('Ctrl Pts',(-37.8437897476033,31.307519227554,2.69934022683663));
#6782=CARTESIAN_POINT('Ctrl Pts',(-37.4116569572008,30.5948955326869,2.64641198709473));
#6783=CARTESIAN_POINT('Ctrl Pts',(-37.3677567303717,29.6468487747117,2.59348374735284));
#6784=CARTESIAN_POINT('Ctrl Pts',(-37.7321840255849,28.89733962636,2.54055550761094));
#6785=CARTESIAN_POINT('Ctrl Pts',(-38.096611320798,28.1478304780083,2.48762726786905));
#6786=CARTESIAN_POINT('Ctrl Pts',(-38.8693661380534,27.5968589392801,2.43469902812715));
#6787=CARTESIAN_POINT('Ctrl Pts',(-39.6967263578976,27.4966274820302,2.38177078838526));
#6788=CARTESIAN_POINT('Ctrl Pts',(-40.5240865777418,27.3963960247803,2.32884254864336));
#6789=CARTESIAN_POINT('Ctrl Pts',(-41.4060522001749,27.7469046490088,2.27591430890147));
#6790=CARTESIAN_POINT('Ctrl Pts',(-41.9389107152419,28.3877113248286,2.22298606915957));
#6791=CARTESIAN_POINT('Ctrl Pts',(-42.3094064064687,28.833263203212,2.18618514693704));
#6792=CARTESIAN_POINT('Ctrl Pts',(-42.5111297881759,29.4191567463233,2.14938422471451));
#6793=CARTESIAN_POINT('Ctrl Pts',(-42.515808333435,30.0021290957888,2.11258330249199));
#6794=CARTESIAN_POINT('Ctrl Pts',(-42.521313086871,30.0008653513074,2.38741669750802));
#6795=CARTESIAN_POINT('Ctrl Pts',(-42.5178102495169,29.2148281860683,2.4373171971363));
#6796=CARTESIAN_POINT('Ctrl Pts',(-42.1208327469498,28.4257395206662,2.48721769676458));
#6797=CARTESIAN_POINT('Ctrl Pts',(-41.4860274785154,27.9627049430877,2.53711819639287));
#6798=CARTESIAN_POINT('Ctrl Pts',(-40.812705053141,27.4715754892061,2.59004643613476));
#6799=CARTESIAN_POINT('Ctrl Pts',(-39.8718186341432,27.3472675187503,2.64297467587666));
#6800=CARTESIAN_POINT('Ctrl Pts',(-39.0940511926965,27.6466819979924,2.69590291561855));
#6801=CARTESIAN_POINT('Ctrl Pts',(-38.3162837512497,27.9460964772345,2.74883115536045));
#6802=CARTESIAN_POINT('Ctrl Pts',(-37.701635287354,28.6692334061744,2.80175939510234));
#6803=CARTESIAN_POINT('Ctrl Pts',(-37.5314560665151,29.485082818627,2.85468763484424));
#6804=CARTESIAN_POINT('Ctrl Pts',(-37.3612768456762,30.3009322310796,2.90761587458613));
#6805=CARTESIAN_POINT('Ctrl Pts',(-37.6355668678942,31.2094941270447,2.96054411432802));
#6806=CARTESIAN_POINT('Ctrl Pts',(-38.2287721370648,31.7948818078934,3.01347235406992));
#6807=CARTESIAN_POINT('Ctrl Pts',(-38.8219774062353,32.380269488742,3.06640059381181));
#6808=CARTESIAN_POINT('Ctrl Pts',(-39.7340979223584,32.6424829544742,3.11932883355371));
#6809=CARTESIAN_POINT('Ctrl Pts',(-40.547618054905,32.4614961544749,3.1722570732956));
#6810=CARTESIAN_POINT('Ctrl Pts',(-41.3611381874516,32.2805093544756,3.2251853130375));
#6811=CARTESIAN_POINT('Ctrl Pts',(-42.0760579364217,31.656322288745,3.27811355277939));
#6812=CARTESIAN_POINT('Ctrl Pts',(-42.3651286906778,30.8746514323181,3.33104179252129));
#6813=CARTESIAN_POINT('Ctrl Pts',(-42.4677603317142,30.5971271184115,3.34983342751686));
#6814=CARTESIAN_POINT('Ctrl Pts',(-42.5167122997757,30.2997514522924,3.36862506251244));
#6815=CARTESIAN_POINT('Ctrl Pts',(-42.5147865997281,30.0017637212727,3.38741669750802));
#6816=CARTESIAN_POINT('Origin',(-40.,30.,5.));
#6817=CARTESIAN_POINT('',(-42.51493238455,29.9981671625222,4.38741669750802));
#6818=CARTESIAN_POINT('',(-42.52066153614,29.998576517643,4.11258330249199));
#6819=CARTESIAN_POINT('',(-42.5175,30.,5.));
#6820=CARTESIAN_POINT('Ctrl Pts',(-42.52066153614,29.998576517643,4.11258330249199));
#6821=CARTESIAN_POINT('Ctrl Pts',(-42.515579438117,30.7497577154419,4.06492819520869));
#6822=CARTESIAN_POINT('Ctrl Pts',(-42.1578861912069,31.5051392898487,4.01727308792539));
#6823=CARTESIAN_POINT('Ctrl Pts',(-41.5708987560698,31.9725937848838,3.96961798064209));
#6824=CARTESIAN_POINT('Ctrl Pts',(-40.91895999308,32.4917730500686,3.9166897409002));
#6825=CARTESIAN_POINT('Ctrl Pts',(-39.9841758787722,32.6557804875304,3.86376150115831));
#6826=CARTESIAN_POINT('Ctrl Pts',(-39.1944361205037,32.3895430478001,3.81083326141641));
#6827=CARTESIAN_POINT('Ctrl Pts',(-38.4046963622352,32.1233056080699,3.75790502167452));
#6828=CARTESIAN_POINT('Ctrl Pts',(-37.760000960006,31.4268232911476,3.70497678193262));
#6829=CARTESIAN_POINT('Ctrl Pts',(-37.5554539093262,30.6189051241564,3.65204854219073));
#6830=CARTESIAN_POINT('Ctrl Pts',(-37.3509068586463,29.8109869571652,3.59912030244883));
#6831=CARTESIAN_POINT('Ctrl Pts',(-37.5865081595159,28.891632940105,3.54619206270694));
#6832=CARTESIAN_POINT('Ctrl Pts',(-38.1544132623102,28.281669782368,3.49326382296504));
#6833=CARTESIAN_POINT('Ctrl Pts',(-38.7223183651046,27.6717066246309,3.44033558322315));
#6834=CARTESIAN_POINT('Ctrl Pts',(-39.6225272698237,27.371134326217,3.38740734348126));
#6835=CARTESIAN_POINT('Ctrl Pts',(-40.4429767859361,27.5175373709795,3.33447910373936));
#6836=CARTESIAN_POINT('Ctrl Pts',(-41.2634263020485,27.663940415742,3.28155086399747));
#6837=CARTESIAN_POINT('Ctrl Pts',(-42.0041164295541,28.257318803681,3.22862262425557));
#6838=CARTESIAN_POINT('Ctrl Pts',(-42.3260023798981,29.0260584850534,3.17569438451368));
#6839=CARTESIAN_POINT('Ctrl Pts',(-42.453940198555,29.3316042159084,3.15465735717311));
#6840=CARTESIAN_POINT('Ctrl Pts',(-42.5157165929052,29.664852996481,3.13362032983255));
#6841=CARTESIAN_POINT('Ctrl Pts',(-42.5141171500829,29.9986698323151,3.11258330249199));
#6842=CARTESIAN_POINT('Ctrl Pts',(-42.5147865997281,30.0017637212727,3.38741669750802));
#6843=CARTESIAN_POINT('Ctrl Pts',(-42.5112884016521,29.4604436394667,3.42155330225433));
#6844=CARTESIAN_POINT('Ctrl Pts',(-42.3398948378532,28.9171037547851,3.45568990700065));
#6845=CARTESIAN_POINT('Ctrl Pts',(-42.0174030796383,28.4870777730195,3.48982651174697));
#6846=CARTESIAN_POINT('Ctrl Pts',(-41.5173849548006,27.8203296172707,3.54275475148886));
#6847=CARTESIAN_POINT('Ctrl Pts',(-40.6541269455829,27.4259879528961,3.59568299123076));
#6848=CARTESIAN_POINT('Ctrl Pts',(-39.8227782752959,27.4845594199695,3.64861123097265));
#6849=CARTESIAN_POINT('Ctrl Pts',(-38.991429605009,27.5431308870429,3.70153947071455));
#6850=CARTESIAN_POINT('Ctrl Pts',(-38.1919902736528,28.0546154855643,3.75446771045644));
#6851=CARTESIAN_POINT('Ctrl Pts',(-37.7903970322367,28.7848853650609,3.80739595019834));
#6852=CARTESIAN_POINT('Ctrl Pts',(-37.3888037908207,29.5151552445575,3.86032418994023));
#6853=CARTESIAN_POINT('Ctrl Pts',(-37.3850566393447,30.4642104050294,3.91325242968213));
#6854=CARTESIAN_POINT('Ctrl Pts',(-37.7808708053848,31.1976286856571,3.96618066942402));
#6855=CARTESIAN_POINT('Ctrl Pts',(-38.1766849714248,31.9310469662847,4.01910890916591));
#6856=CARTESIAN_POINT('Ctrl Pts',(-38.9720604549807,32.4488283670683,4.07203714890781));
#6857=CARTESIAN_POINT('Ctrl Pts',(-39.8029206979638,32.513962728424,4.1249653886497));
#6858=CARTESIAN_POINT('Ctrl Pts',(-40.6337809409469,32.5790970897796,4.1778936283916));
#6859=CARTESIAN_POINT('Ctrl Pts',(-41.5001259433573,32.1915844117074,4.23082186813349));
#6860=CARTESIAN_POINT('Ctrl Pts',(-42.005393435983,31.5288054219173,4.28375010787539));
#6861=CARTESIAN_POINT('Ctrl Pts',(-42.3352700013614,31.0960935218884,4.31830563775293));
#6862=CARTESIAN_POINT('Ctrl Pts',(-42.5112387594207,30.5460504856982,4.35286116763047));
#6863=CARTESIAN_POINT('Ctrl Pts',(-42.51493238455,29.9981671625222,4.38741669750802));
#6864=CARTESIAN_POINT('Origin',(-40.,30.,5.));
#6865=CARTESIAN_POINT('',(-42.5214025534547,29.9992487949168,5.38741669750802));
#6866=CARTESIAN_POINT('',(-42.5184255606712,30.0022201831731,5.11258330249199));
#6867=CARTESIAN_POINT('',(-42.5175,30.,5.));
#6868=CARTESIAN_POINT('Ctrl Pts',(-42.5184255606712,30.0022201831731,5.11258330249199));
#6869=CARTESIAN_POINT('Ctrl Pts',(-42.5199489469804,30.1679668215771,5.10209254006862));
#6870=CARTESIAN_POINT('Ctrl Pts',(-42.5049858464185,30.3334397470291,5.09160177764525));
#6871=CARTESIAN_POINT('Ctrl Pts',(-42.4725330539849,30.4954083555317,5.08111101522188));
#6872=CARTESIAN_POINT('Ctrl Pts',(-42.3088014671944,31.3125761642691,5.02818277547999));
#6873=CARTESIAN_POINT('Ctrl Pts',(-41.6998823865396,32.0405441122082,4.97525453573809));
#6874=CARTESIAN_POINT('Ctrl Pts',(-40.9245034917662,32.3460908838952,4.9223262959962));
#6875=CARTESIAN_POINT('Ctrl Pts',(-40.1491245969927,32.6516376555822,4.8693980562543));
#6876=CARTESIAN_POINT('Ctrl Pts',(-39.2072858881007,32.534763251017,4.81646981651241));
#6877=CARTESIAN_POINT('Ctrl Pts',(-38.5301062548807,32.0489659635609,4.76354157677051));
#6878=CARTESIAN_POINT('Ctrl Pts',(-37.8529266216607,31.5631686761048,4.71061333702862));
#6879=CARTESIAN_POINT('Ctrl Pts',(-37.4404060641128,30.7084485057578,4.65768509728672));
#6880=CARTESIAN_POINT('Ctrl Pts',(-37.4813724602034,29.8760465508429,4.60475685754483));
#6881=CARTESIAN_POINT('Ctrl Pts',(-37.522338856294,29.043644595928,4.55182861780293));
#6882=CARTESIAN_POINT('Ctrl Pts',(-38.0167922060231,28.2335608564452,4.49890037806104));
#6883=CARTESIAN_POINT('Ctrl Pts',(-38.7384005725339,27.8166044732056,4.44597213831915));
#6884=CARTESIAN_POINT('Ctrl Pts',(-39.4600089390446,27.399648089966,4.39304389857725));
#6885=CARTESIAN_POINT('Ctrl Pts',(-40.408772322337,27.3758190629697,4.34011565883535));
#6886=CARTESIAN_POINT('Ctrl Pts',(-41.1504021201121,27.7560249324566,4.28718741909346));
#6887=CARTESIAN_POINT('Ctrl Pts',(-41.8920319178872,28.1362308019434,4.23425917935157));
#6888=CARTESIAN_POINT('Ctrl Pts',(-42.4265281301451,28.9204715679134,4.18133093960967));
#6889=CARTESIAN_POINT('Ctrl Pts',(-42.5092295304381,29.7497674973523,4.12840269986778));
#6890=CARTESIAN_POINT('Ctrl Pts',(-42.5174689020927,29.8323885575771,4.12312956740918));
#6891=CARTESIAN_POINT('Ctrl Pts',(-42.5212238804001,29.9154568231924,4.11785643495059));
#6892=CARTESIAN_POINT('Ctrl Pts',(-42.52066153614,29.998576517643,4.11258330249199));
#6893=CARTESIAN_POINT('Ctrl Pts',(-42.51493238455,29.9981671625222,4.38741669750802));
#6894=CARTESIAN_POINT('Ctrl Pts',(-42.5168962352879,29.7068649781279,4.40578940737237));
#6895=CARTESIAN_POINT('Ctrl Pts',(-42.4701595306737,29.4161733242344,4.42416211723672));
#6896=CARTESIAN_POINT('Ctrl Pts',(-42.3719616108191,29.1440520062763,4.44253482710107));
#6897=CARTESIAN_POINT('Ctrl Pts',(-42.0890723101885,28.3601228819334,4.49546306684297));
#6898=CARTESIAN_POINT('Ctrl Pts',(-41.3791037260861,27.7303099347556,4.54839130658486));
#6899=CARTESIAN_POINT('Ctrl Pts',(-40.5670381138294,27.5429048393202,4.60131954632675));
#6900=CARTESIAN_POINT('Ctrl Pts',(-39.7549725015727,27.3554997438847,4.65424778606865));
#6901=CARTESIAN_POINT('Ctrl Pts',(-38.8408098611616,27.6105025001917,4.70717602581054));
#6902=CARTESIAN_POINT('Ctrl Pts',(-38.243000590635,28.1911877027572,4.76010426555244));
#6903=CARTESIAN_POINT('Ctrl Pts',(-37.6451913201083,28.7718729053228,4.81303250529433));
#6904=CARTESIAN_POINT('Ctrl Pts',(-37.363735419466,29.678240554147,4.86596074503623));
#6905=CARTESIAN_POINT('Ctrl Pts',(-37.5274670025151,30.4954083442112,4.91888898477812));
#6906=CARTESIAN_POINT('Ctrl Pts',(-37.6911985855641,31.3125761342754,4.97181722452002));
#6907=CARTESIAN_POINT('Ctrl Pts',(-38.3001176523045,32.0405440655797,5.02474546426191));
#6908=CARTESIAN_POINT('Ctrl Pts',(-39.0754965293597,32.3460908302846,5.07767370400381));
#6909=CARTESIAN_POINT('Ctrl Pts',(-39.850875406415,32.6516375949895,5.1306019437457));
#6910=CARTESIAN_POINT('Ctrl Pts',(-40.792714093785,32.534763193095,5.18353018348759));
#6911=CARTESIAN_POINT('Ctrl Pts',(-41.4698937115307,32.0489659167399,5.23645842322949));
#6912=CARTESIAN_POINT('Ctrl Pts',(-42.1136953756329,31.5871134233426,5.286777847989));
#6913=CARTESIAN_POINT('Ctrl Pts',(-42.5182849001928,30.7918099348553,5.33709727274851));
#6914=CARTESIAN_POINT('Ctrl Pts',(-42.5214025534547,29.9992487949168,5.38741669750802));
#6915=CARTESIAN_POINT('Origin',(-40.,30.,5.));
#6916=CARTESIAN_POINT('',(-42.5171492932468,30.0023011681775,6.38741669750801));
#6917=CARTESIAN_POINT('',(-42.51341458009,30.0000546151609,6.11258330249199));
#6918=CARTESIAN_POINT('',(-42.5175,30.,5.));
#6919=CARTESIAN_POINT('Ctrl Pts',(-42.51341458009,30.0000546151609,6.11258330249199));
#6920=CARTESIAN_POINT('Ctrl Pts',(-42.5134952326931,30.4169561760255,6.08632864518665));
#6921=CARTESIAN_POINT('Ctrl Pts',(-42.4154699053225,30.8338220541732,6.06007398788132));
#6922=CARTESIAN_POINT('Ctrl Pts',(-42.2191292453247,31.1976287130241,6.03381933057598));
#6923=CARTESIAN_POINT('Ctrl Pts',(-41.8233150702399,31.9310470104112,5.98089109083409));
#6924=CARTESIAN_POINT('Ctrl Pts',(-41.0279395685088,32.4488284230266,5.9279628510922));
#6925=CARTESIAN_POINT('Ctrl Pts',(-40.1970793065397,32.5139627858706,5.8750346113503));
#6926=CARTESIAN_POINT('Ctrl Pts',(-39.3662190445705,32.5790971487147,5.82210637160841));
#6927=CARTESIAN_POINT('Ctrl Pts',(-38.4998740223633,32.1915844617874,5.76917813186651));
#6928=CARTESIAN_POINT('Ctrl Pts',(-37.9946065181917,31.5288054568521,5.71624989212461));
#6929=CARTESIAN_POINT('Ctrl Pts',(-37.4893390140201,30.8660264519168,5.66332165238272));
#6930=CARTESIAN_POINT('Ctrl Pts',(-37.3451490278841,29.9279811289735,5.61039341264083));
#6931=CARTESIAN_POINT('Ctrl Pts',(-37.6280383349791,29.144051986717,5.55746517289893));
#6932=CARTESIAN_POINT('Ctrl Pts',(-37.910927642074,28.3601228444605,5.50453693315704));
#6933=CARTESIAN_POINT('Ctrl Pts',(-38.6208962423999,27.7303098828908,5.45160869341514));
#6934=CARTESIAN_POINT('Ctrl Pts',(-39.4329618732132,27.542904783173,5.39868045367325));
#6935=CARTESIAN_POINT('Ctrl Pts',(-40.2450275040264,27.3554996834551,5.34575221393135));
#6936=CARTESIAN_POINT('Ctrl Pts',(-41.159190165327,27.6105024455891,5.29282397418946));
#6937=CARTESIAN_POINT('Ctrl Pts',(-41.7569994495142,28.1911876614239,5.23989573444757));
#6938=CARTESIAN_POINT('Ctrl Pts',(-42.2363185816489,28.6567768402132,5.19745825712904));
#6939=CARTESIAN_POINT('Ctrl Pts',(-42.5122631227723,29.3317380080906,5.15502077981052));
#6940=CARTESIAN_POINT('Ctrl Pts',(-42.5184255606712,30.0022201831731,5.11258330249199));
#6941=CARTESIAN_POINT('Ctrl Pts',(-42.5214025534547,29.9992487949168,5.38741669750802));
#6942=CARTESIAN_POINT('Ctrl Pts',(-42.5215641884611,29.9581583932238,5.3900255124904));
#6943=CARTESIAN_POINT('Ctrl Pts',(-42.5206467019638,29.9170753627254,5.39263432747279));
#6944=CARTESIAN_POINT('Ctrl Pts',(-42.5186274822434,29.8760465536754,5.39524314245517));
#6945=CARTESIAN_POINT('Ctrl Pts',(-42.4776610870889,29.0436446177817,5.44817138219707));
#6946=CARTESIAN_POINT('Ctrl Pts',(-41.9832077486585,28.2335608968101,5.50109962193896));
#6947=CARTESIAN_POINT('Ctrl Pts',(-41.2615993986372,27.8166045230985,5.55402786168086));
#6948=CARTESIAN_POINT('Ctrl Pts',(-40.539991048616,27.3996481493868,5.60695610142275));
#6949=CARTESIAN_POINT('Ctrl Pts',(-39.5912276870039,27.375819122935,5.65988434116464));
#6950=CARTESIAN_POINT('Ctrl Pts',(-38.8495979061758,27.7560249837337,5.71281258090654));
#6951=CARTESIAN_POINT('Ctrl Pts',(-38.1079681253477,28.1362308445325,5.76574082064843));
#6952=CARTESIAN_POINT('Ctrl Pts',(-37.5734719253036,28.9204715925817,5.81866906039033));
#6953=CARTESIAN_POINT('Ctrl Pts',(-37.4907705269003,29.7497675030704,5.87159730013222));
#6954=CARTESIAN_POINT('Ctrl Pts',(-37.4080691284971,30.5790634135591,5.92452553987411));
#6955=CARTESIAN_POINT('Ctrl Pts',(-37.7771625317346,31.4534144864871,5.97745377961601));
#6956=CARTESIAN_POINT('Ctrl Pts',(-38.4291012798269,31.9725937398081,6.0303820193579));
#6957=CARTESIAN_POINT('Ctrl Pts',(-39.0810400279192,32.491772993129,6.0833102590998));
#6958=CARTESIAN_POINT('Ctrl Pts',(-40.0158241208662,32.6557804268428,6.13623849884169));
#6959=CARTESIAN_POINT('Ctrl Pts',(-40.8055638610884,32.3895429931965,6.18916673858359));
#6960=CARTESIAN_POINT('Ctrl Pts',(-41.5953036013105,32.1233055595501,6.24209497832548));
#6961=CARTESIAN_POINT('Ctrl Pts',(-42.2399989888077,31.4268232585436,6.29502321806738));
#6962=CARTESIAN_POINT('Ctrl Pts',(-42.4445460348134,30.6189051100139,6.34795145780927));
#6963=CARTESIAN_POINT('Ctrl Pts',(-42.4953852984381,30.4181006274153,6.36110653770885));
#6964=CARTESIAN_POINT('Ctrl Pts',(-42.5190344405339,30.2104122060369,6.37426161760843));
#6965=CARTESIAN_POINT('Ctrl Pts',(-42.5171492932468,30.0023011681775,6.38741669750801));
#6966=CARTESIAN_POINT('Origin',(-40.,30.,5.));
#6967=CARTESIAN_POINT('',(-42.5135601364305,29.999367791574,7.38741669750801));
#6968=CARTESIAN_POINT('',(-42.5182250179402,29.9977519260729,7.11258330249199));
#6969=CARTESIAN_POINT('',(-42.5175,30.,5.));
#6970=CARTESIAN_POINT('Ctrl Pts',(-42.5182250179402,29.9977519260729,7.11258330249199));
#6971=CARTESIAN_POINT('Ctrl Pts',(-42.5120991076497,30.6617513777343,7.07056475030469));
#6972=CARTESIAN_POINT('Ctrl Pts',(-42.2421603820176,31.3301555799156,7.02854619811739));
#6973=CARTESIAN_POINT('Ctrl Pts',(-41.7712279034101,31.7948818489091,6.98652764593008));
#6974=CARTESIAN_POINT('Ctrl Pts',(-41.1780226206846,32.3802695431352,6.93359940618819));
#6975=CARTESIAN_POINT('Ctrl Pts',(-40.2659020837177,32.6424830148576,6.8806711664463));
#6976=CARTESIAN_POINT('Ctrl Pts',(-39.4523819325812,32.4614962107223,6.8277429267044));
#6977=CARTESIAN_POINT('Ctrl Pts',(-38.6388617814446,32.2805094065869,6.77481468696251));
#6978=CARTESIAN_POINT('Ctrl Pts',(-37.9239420161383,31.6563223265937,6.72188644722061));
#6979=CARTESIAN_POINT('Ctrl Pts',(-37.6348712552767,30.8746514523051,6.66895820747871));
#6980=CARTESIAN_POINT('Ctrl Pts',(-37.3458004944151,30.0929805780164,6.61602996773682));
#6981=CARTESIAN_POINT('Ctrl Pts',(-37.4825787379982,29.1538259094324,6.56310172799493));
#6982=CARTESIAN_POINT('Ctrl Pts',(-37.9825968742618,28.4870777384476,6.51017348825303));
#6983=CARTESIAN_POINT('Ctrl Pts',(-38.4826150105254,27.8203295674628,6.45724524851114));
#6984=CARTESIAN_POINT('Ctrl Pts',(-39.3458730394696,27.4259878940772,6.40431700876925));
#6985=CARTESIAN_POINT('Ctrl Pts',(-40.1772217287538,27.4845593624891,6.35138876902735));
#6986=CARTESIAN_POINT('Ctrl Pts',(-41.008570418038,27.5431308309009,6.29846052928545));
#6987=CARTESIAN_POINT('Ctrl Pts',(-41.8080097676621,28.0546154411102,6.24553228954356));
#6988=CARTESIAN_POINT('Ctrl Pts',(-42.209603018255,28.7848853372942,6.19260404980166));
#6989=CARTESIAN_POINT('Ctrl Pts',(-42.4119889416843,29.1529103154872,6.1659304673651));
#6990=CARTESIAN_POINT('Ctrl Pts',(-42.5133326405761,29.5765008805862,6.13925688492855));
#6991=CARTESIAN_POINT('Ctrl Pts',(-42.51341458009,30.0000546151609,6.11258330249199));
#6992=CARTESIAN_POINT('Ctrl Pts',(-42.5171492932468,30.0023011681775,6.38741669750801));
#6993=CARTESIAN_POINT('Ctrl Pts',(-42.5114497258593,29.3730968123762,6.42718985735033));
#6994=CARTESIAN_POINT('Ctrl Pts',(-42.2723414869604,28.7400293237536,6.46696301719264));
#6995=CARTESIAN_POINT('Ctrl Pts',(-41.8455866955162,28.2816698216331,6.50673617703495));
#6996=CARTESIAN_POINT('Ctrl Pts',(-41.277681605699,27.6717066778348,6.55966441677685));
#6997=CARTESIAN_POINT('Ctrl Pts',(-40.3774727215505,27.371134386291,6.61259265651875));
#6998=CARTESIAN_POINT('Ctrl Pts',(-39.5570232241863,27.5175374277073,6.66552089626064));
#6999=CARTESIAN_POINT('Ctrl Pts',(-38.7365737268221,27.6639404691235,6.71844913600254));
#7000=CARTESIAN_POINT('Ctrl Pts',(-37.9958836162423,28.2573188434998,6.77137737574443));
#7001=CARTESIAN_POINT('Ctrl Pts',(-37.6739976732536,29.0260585073073,6.82430561548633));
#7002=CARTESIAN_POINT('Ctrl Pts',(-37.3521117302649,29.7947981711147,6.87723385522822));
#7003=CARTESIAN_POINT('Ctrl Pts',(-37.4490299548673,30.7388991243533,6.93016209497011));
#7004=CARTESIAN_POINT('Ctrl Pts',(-37.9203888292803,31.4262069410312,6.983090334712));
#7005=CARTESIAN_POINT('Ctrl Pts',(-38.3917477036933,32.1135147577091,7.0360185744539));
#7006=CARTESIAN_POINT('Ctrl Pts',(-39.2375472279169,32.5440294378263,7.0889468141958));
#7007=CARTESIAN_POINT('Ctrl Pts',(-40.0706296576422,32.5206864674694,7.14187505393769));
#7008=CARTESIAN_POINT('Ctrl Pts',(-40.9037120873676,32.4973434971125,7.19480329367959));
#7009=CARTESIAN_POINT('Ctrl Pts',(-41.7240774225947,32.0201428762815,7.24773153342148));
#7010=CARTESIAN_POINT('Ctrl Pts',(-42.1562102031238,31.3075191976881,7.30065977316337));
#7011=CARTESIAN_POINT('Ctrl Pts',(-42.3923192640589,30.9181552911899,7.32957874794492));
#7012=CARTESIAN_POINT('Ctrl Pts',(-42.5125284857968,30.4585100695166,7.35849772272647));
#7013=CARTESIAN_POINT('Ctrl Pts',(-42.5135601364305,29.999367791574,7.38741669750801));
#7014=CARTESIAN_POINT('Origin',(-40.,30.,5.));
#7015=CARTESIAN_POINT('',(-42.5194677947045,29.9980220285566,8.38741669750802));
#7016=CARTESIAN_POINT('',(-42.5208028517601,30.0013273486611,8.11258330249199));
#7017=CARTESIAN_POINT('',(-42.5175,30.,5.));
#7018=CARTESIAN_POINT('Ctrl Pts',(-42.5208028517601,30.0013273486611,8.11258330249199));
#7019=CARTESIAN_POINT('Ctrl Pts',(-42.5212922101133,30.0778322922101,8.10772909516461));
#7020=CARTESIAN_POINT('Ctrl Pts',(-42.5181112889522,30.1542959881703,8.10287488783724));
#7021=CARTESIAN_POINT('Ctrl Pts',(-42.5111273223559,30.2304107303999,8.09802068050987));
#7022=CARTESIAN_POINT('Ctrl Pts',(-42.4349770812501,31.0603339398802,8.04509244076797));
#7023=CARTESIAN_POINT('Ctrl Pts',(-41.9066901274328,31.8487707155565,7.99216420102608));
#7024=CARTESIAN_POINT('Ctrl Pts',(-41.1680857014233,32.2348209458145,7.93923596128418));
#7025=CARTESIAN_POINT('Ctrl Pts',(-40.4294812754137,32.6208711760725,7.88630772154229));
#7026=CARTESIAN_POINT('Ctrl Pts',(-39.4805593772119,32.6045348609122,7.83337948180039));
#7027=CARTESIAN_POINT('Ctrl Pts',(-38.7556810423998,32.1932896582907,7.7804512420585));
#7028=CARTESIAN_POINT('Ctrl Pts',(-38.0308027075876,31.7820444556692,7.72752300231661));
#7029=CARTESIAN_POINT('Ctrl Pts',(-37.529967936165,30.9758903655866,7.67459476257471));
#7030=CARTESIAN_POINT('Ctrl Pts',(-37.4824297709596,30.1438378420785,7.62166652283282));
#7031=CARTESIAN_POINT('Ctrl Pts',(-37.4348916057543,29.3117853185706,7.56873828309092));
#7032=CARTESIAN_POINT('Ctrl Pts',(-37.8406500467662,28.4538343616372,7.51581004334903));
#7033=CARTESIAN_POINT('Ctrl Pts',(-38.5139724875241,27.9627048965278,7.46288180360713));
#7034=CARTESIAN_POINT('Ctrl Pts',(-39.187294928282,27.4715754314184,7.40995356386524));
#7035=CARTESIAN_POINT('Ctrl Pts',(-40.1281813687861,27.3472674581329,7.35702532412334));
#7036=CARTESIAN_POINT('Ctrl Pts',(-40.905948828007,27.6466819442195,7.30409708438145));
#7037=CARTESIAN_POINT('Ctrl Pts',(-41.683716287228,27.9460964303061,7.25116884463956));
#7038=CARTESIAN_POINT('Ctrl Pts',(-42.2983647651659,28.6692333757648,7.19824060489766));
#7039=CARTESIAN_POINT('Ctrl Pts',(-42.4685439898928,29.485082806859,7.14531236515577));
#7040=CARTESIAN_POINT('Ctrl Pts',(-42.5036217136015,29.6532475224859,7.13440267760118));
#7041=CARTESIAN_POINT('Ctrl Pts',(-42.519815547927,29.8253512559651,7.12349299004658));
#7042=CARTESIAN_POINT('Ctrl Pts',(-42.5182250179402,29.9977519260729,7.11258330249199));
#7043=CARTESIAN_POINT('Ctrl Pts',(-42.5135601364305,29.999367791574,7.38741669750801));
#7044=CARTESIAN_POINT('Ctrl Pts',(-42.5144166389034,29.6181762490351,7.41142596246836));
#7045=CARTESIAN_POINT('Ctrl Pts',(-42.4331271313634,29.2373313725707,7.43543522742871));
#7046=CARTESIAN_POINT('Ctrl Pts',(-42.2678159225957,28.8973396515338,7.45944449238906));
#7047=CARTESIAN_POINT('Ctrl Pts',(-41.9033886357073,28.1478305203288,7.51237273213095));
#7048=CARTESIAN_POINT('Ctrl Pts',(-41.1306338360994,27.5968589942747,7.56530097187285));
#7049=CARTESIAN_POINT('Ctrl Pts',(-40.303273635167,27.4966275392785,7.61822921161474));
#7050=CARTESIAN_POINT('Ctrl Pts',(-39.4759134342346,27.3963960842823,7.67115745135664));
#7051=CARTESIAN_POINT('Ctrl Pts',(-38.5939478319776,27.746904700344,7.72408569109853));
#7052=CARTESIAN_POINT('Ctrl Pts',(-38.0610893290751,28.3877113615891,7.77701393084042));
#7053=CARTESIAN_POINT('Ctrl Pts',(-37.5282308261726,29.0285180228342,7.82994217058231));
#7054=CARTESIAN_POINT('Ctrl Pts',(-37.3444794226246,29.9596227292627,7.88287041032422));
#7055=CARTESIAN_POINT('Ctrl Pts',(-37.5939457439436,30.7548191971487,7.93579865006611));
#7056=CARTESIAN_POINT('Ctrl Pts',(-37.8434120652626,31.5500156650348,7.98872688980801));
#7057=CARTESIAN_POINT('Ctrl Pts',(-38.5260961114487,32.2093038943785,8.04165512954989));
#7058=CARTESIAN_POINT('Ctrl Pts',(-39.3295050223605,32.4309017309935,8.09458336929179));
#7059=CARTESIAN_POINT('Ctrl Pts',(-40.1329139332723,32.6524995676084,8.14751160903368));
#7060=CARTESIAN_POINT('Ctrl Pts',(-41.0570477089098,32.4364070114946,8.20043984877558));
#7061=CARTESIAN_POINT('Ctrl Pts',(-41.6788915002102,31.8815354756122,8.25336808851748));
#7062=CARTESIAN_POINT('Ctrl Pts',(-42.2038620114768,31.4131040174958,8.29805095818099));
#7063=CARTESIAN_POINT('Ctrl Pts',(-42.5133902258015,30.7032245282214,8.34273382784451));
#7064=CARTESIAN_POINT('Ctrl Pts',(-42.5194677947045,29.9980220285566,8.38741669750802));
#7065=CARTESIAN_POINT('Origin',(-40.,30.,5.));
#7066=CARTESIAN_POINT('',(-42.5197815649842,30.0018165623494,9.38741669750802));
#7067=CARTESIAN_POINT('',(-42.5142224421888,30.0014129136195,9.11258330249199));
#7068=CARTESIAN_POINT('',(-42.5175,30.,5.));
#7069=CARTESIAN_POINT('',(-38.0865340033349,31.635987203375,10.));
#7070=CARTESIAN_POINT('Ctrl Pts',(-42.5197815649842,30.0018165623494,9.38741669750802));
#7071=CARTESIAN_POINT('Ctrl Pts',(-42.513858141005,29.2855376666819,9.43282641244632));
#7072=CARTESIAN_POINT('Ctrl Pts',(-42.1929705189018,28.5647530629107,9.47823612738464));
#7073=CARTESIAN_POINT('Ctrl Pts',(-41.6529744178988,28.0958628304862,9.52364584232295));
#7074=CARTESIAN_POINT('Ctrl Pts',(-41.0235707069879,27.5493380467894,9.57657408206484));
#7075=CARTESIAN_POINT('Ctrl Pts',(-40.0964959908271,27.3450257192792,9.62950232180674));
#7076=CARTESIAN_POINT('Ctrl Pts',(-39.2962220007402,27.5780866216694,9.68243056154863));
#7077=CARTESIAN_POINT('Ctrl Pts',(-38.4959480106534,27.8111475240597,9.73535880129053));
#7078=CARTESIAN_POINT('Ctrl Pts',(-37.8224747466407,28.4815816563505,9.78828704103242));
#7079=CARTESIAN_POINT('Ctrl Pts',(-37.5841061119589,29.2787069994738,9.84121528077432));
#7080=CARTESIAN_POINT('Ctrl Pts',(-37.3457374772771,30.0758323425971,9.89414352051621));
#7081=CARTESIAN_POINT('Ctrl Pts',(-37.5424734719262,30.999648896553,9.94707176025811));
#7082=CARTESIAN_POINT('Ctrl Pts',(-38.0865340033349,31.635987203375,10.));
#7083=CARTESIAN_POINT('',(-41.9171062441644,31.638757234455,9.99999999999999));
#7084=CARTESIAN_POINT('Origin',(-40.,30.,10.));
#7085=CARTESIAN_POINT('Ctrl Pts',(-41.9171091880766,31.6387594746126,9.99999999999999));
#7086=CARTESIAN_POINT('Ctrl Pts',(-41.3863009439606,32.2578634975499,9.94821753066412));
#7087=CARTESIAN_POINT('Ctrl Pts',(-40.5267000509608,32.5973561981228,9.89643506132826));
#7088=CARTESIAN_POINT('Ctrl Pts',(-39.7163628878231,32.5055165856408,9.84465259199239));
#7089=CARTESIAN_POINT('Ctrl Pts',(-38.8880957118387,32.4116448740444,9.7917243522505));
#7090=CARTESIAN_POINT('Ctrl Pts',(-38.111296463077,31.8671418326788,9.7387961125086));
#7091=CARTESIAN_POINT('Ctrl Pts',(-37.7410325214101,31.1206210243586,9.6858678727667));
#7092=CARTESIAN_POINT('Ctrl Pts',(-37.3707685797432,30.3741002160383,9.6329396330248));
#7093=CARTESIAN_POINT('Ctrl Pts',(-37.4070399451711,29.4255616407633,9.58001139328291));
#7094=CARTESIAN_POINT('Ctrl Pts',(-37.8334967847582,28.7095042189904,9.52708315354102));
#7095=CARTESIAN_POINT('Ctrl Pts',(-38.2599536243453,27.9934467972176,9.47415491379912));
#7096=CARTESIAN_POINT('Ctrl Pts',(-39.0765959380917,27.509870528947,9.42122667405723));
#7097=CARTESIAN_POINT('Ctrl Pts',(-39.9094857441256,27.4799717114424,9.36829843431534));
#7098=CARTESIAN_POINT('Ctrl Pts',(-40.7423755501596,27.4500728939378,9.31537019457344));
#7099=CARTESIAN_POINT('Ctrl Pts',(-41.5915128484811,27.8738515271992,9.26244195483155));
#7100=CARTESIAN_POINT('Ctrl Pts',(-42.0682755018096,28.5574049250838,9.20951371508965));
#7101=CARTESIAN_POINT('Ctrl Pts',(-42.3593161064952,28.9746813054093,9.1772035775571));
#7102=CARTESIAN_POINT('Ctrl Pts',(-42.5115907928592,29.4887631053692,9.14489344002455));
#7103=CARTESIAN_POINT('Ctrl Pts',(-42.5142224421888,30.0014129136195,9.11258330249199));
#7104=CARTESIAN_POINT('Origin',(-40.,-30.,5.));
#7105=CARTESIAN_POINT('',(-42.5134504848964,-29.9993943075263,0.38741669750801));
#7106=CARTESIAN_POINT('',(-42.5156173960267,-30.0035024211729,0.112583302491982));
#7107=CARTESIAN_POINT('',(-42.5175,-30.,5.));
#7108=CARTESIAN_POINT('',(-41.9134659966651,-28.364012796625,0.));
#7109=CARTESIAN_POINT('Ctrl Pts',(-42.5156173960267,-30.0035024211729,0.112583302491982));
#7110=CARTESIAN_POINT('Ctrl Pts',(-42.5103683909667,-29.4109031495499,0.0750555349946548));
#7111=CARTESIAN_POINT('Ctrl Pts',(-42.2992218280841,-28.8151964396956,0.0375277674973275));
#7112=CARTESIAN_POINT('Ctrl Pts',(-41.9134659966651,-28.364012796625,0.));
#7113=CARTESIAN_POINT('',(-38.0828936690615,-28.3612428482559,1.02151810828812E-14));
#7114=CARTESIAN_POINT('Origin',(-40.,-30.,0.));
#7115=CARTESIAN_POINT('Ctrl Pts',(-38.0828907224,-28.3612406061267,6.83481049534862E-15));
#7116=CARTESIAN_POINT('Ctrl Pts',(-38.6136989387411,-27.7421367124245,0.051782469335876));
#7117=CARTESIAN_POINT('Ctrl Pts',(-39.4732999017946,-27.4026436690207,0.103564938671745));
#7118=CARTESIAN_POINT('Ctrl Pts',(-40.283637116215,-27.4944832126233,0.155347408007614));
#7119=CARTESIAN_POINT('Ctrl Pts',(-41.1119043446168,-27.5883548538164,0.208275647749507));
#7120=CARTESIAN_POINT('Ctrl Pts',(-41.888703626185,-28.1328581109876,0.261203887491401));
#7121=CARTESIAN_POINT('Ctrl Pts',(-42.2589675775206,-28.8793789907236,0.314132127233294));
#7122=CARTESIAN_POINT('Ctrl Pts',(-42.4298570352352,-29.223923869723,0.338560317324866));
#7123=CARTESIAN_POINT('Ctrl Pts',(-42.514148869307,-29.6115012842663,0.362988507416438));
#7124=CARTESIAN_POINT('Ctrl Pts',(-42.5134504848964,-29.9993943075263,0.38741669750801));
#7125=CARTESIAN_POINT('Origin',(-40.,-30.,5.));
#7126=CARTESIAN_POINT('',(-42.517348422246,-30.0023034643409,1.38741669750801));
#7127=CARTESIAN_POINT('',(-42.5216691698492,-29.9998787127942,1.11258330249199));
#7128=CARTESIAN_POINT('',(-42.5175,-30.,5.));
#7129=CARTESIAN_POINT('Ctrl Pts',(-42.5216691698492,-29.9998787127942,1.11258330249199));
#7130=CARTESIAN_POINT('Ctrl Pts',(-42.5216727213969,-29.9941563074997,1.11221987985459));
#7131=CARTESIAN_POINT('Ctrl Pts',(-42.5216549338522,-29.9884339268551,1.11185645721719));
#7132=CARTESIAN_POINT('Ctrl Pts',(-42.5216157407844,-29.9827116948348,1.11149303457979));
#7133=CARTESIAN_POINT('Ctrl Pts',(-42.5159077306748,-29.1493357928889,1.0585647948379));
#7134=CARTESIAN_POINT('Ctrl Pts',(-42.0561778285,-28.3191122866127,1.005636555096));
#7135=CARTESIAN_POINT('Ctrl Pts',(-41.352855734795,-27.8719685956743,0.952708315354107));
#7136=CARTESIAN_POINT('Ctrl Pts',(-40.6495336410899,-27.4248249047359,0.899780075612213));
#7137=CARTESIAN_POINT('Ctrl Pts',(-39.7026193558544,-27.3607610291354,0.846851835870318));
#7138=CARTESIAN_POINT('Ctrl Pts',(-38.9455707745702,-27.709302480843,0.793923596128424));
#7139=CARTESIAN_POINT('Ctrl Pts',(-38.188522193286,-28.0578439325505,0.740995356386529));
#7140=CARTESIAN_POINT('Ctrl Pts',(-37.621339315953,-28.818990711566,0.688067116644635));
#7141=CARTESIAN_POINT('Ctrl Pts',(-37.5036141315071,-29.6439329244633,0.63513887690274));
#7142=CARTESIAN_POINT('Ctrl Pts',(-37.3858889470612,-30.4688751373606,0.582210637160846));
#7143=CARTESIAN_POINT('Ctrl Pts',(-37.7176214555024,-31.3576127841396,0.529282397418952));
#7144=CARTESIAN_POINT('Ctrl Pts',(-38.3470253385022,-31.904137509153,0.476354157677058));
#7145=CARTESIAN_POINT('Ctrl Pts',(-38.9764292215021,-32.4506622341664,0.423425917935163));
#7146=CARTESIAN_POINT('Ctrl Pts',(-39.9035044790606,-32.6549740374143,0.370497678193268));
#7147=CARTESIAN_POINT('Ctrl Pts',(-40.7037782325491,-32.4219133590322,0.317569438451373));
#7148=CARTESIAN_POINT('Ctrl Pts',(-41.5040519860376,-32.1888526806501,0.264641198709479));
#7149=CARTESIAN_POINT('Ctrl Pts',(-42.177524235456,-31.5184195206382,0.211712958967585));
#7150=CARTESIAN_POINT('Ctrl Pts',(-42.415892870965,-30.7212941263374,0.158784719225691));
#7151=CARTESIAN_POINT('Ctrl Pts',(-42.4852507331013,-30.4893554189435,0.143384246981121));
#7152=CARTESIAN_POINT('Ctrl Pts',(-42.5177714585284,-30.2466905787268,0.127983774736552));
#7153=CARTESIAN_POINT('Ctrl Pts',(-42.5156173960267,-30.0035024211729,0.112583302491982));
#7154=CARTESIAN_POINT('Ctrl Pts',(-42.5134504848964,-29.9993943075263,0.38741669750801));
#7155=CARTESIAN_POINT('Ctrl Pts',(-42.5126356889454,-30.4519440208077,0.415916747158333));
#7156=CARTESIAN_POINT('Ctrl Pts',(-42.3961357474936,-30.9049233275291,0.444416796808655));
#7157=CARTESIAN_POINT('Ctrl Pts',(-42.1665032932827,-31.2904957986896,0.472916846458978));
#7158=CARTESIAN_POINT('Ctrl Pts',(-41.7400464366065,-32.0065532246186,0.525845086200871));
#7159=CARTESIAN_POINT('Ctrl Pts',(-40.9234041021512,-32.4901295741756,0.578773325942766));
#7160=CARTESIAN_POINT('Ctrl Pts',(-40.0905142646775,-32.5200284066574,0.631701565684659));
#7161=CARTESIAN_POINT('Ctrl Pts',(-39.2576244272039,-32.5499272391393,0.684629805426554));
#7162=CARTESIAN_POINT('Ctrl Pts',(-38.4084870867119,-32.126148554546,0.737558045168449));
#7163=CARTESIAN_POINT('Ctrl Pts',(-37.9317244130836,-31.4425951218629,0.790486284910343));
#7164=CARTESIAN_POINT('Ctrl Pts',(-37.4549617394553,-30.7590416891798,0.843414524652238));
#7165=CARTESIAN_POINT('Ctrl Pts',(-37.3505737326908,-29.8157135084069,0.896342764394131));
#7166=CARTESIAN_POINT('Ctrl Pts',(-37.6663749029378,-29.0444505300205,0.949271004136026));
#7167=CARTESIAN_POINT('Ctrl Pts',(-37.9821760731849,-28.2731875516341,1.00219924387792));
#7168=CARTESIAN_POINT('Ctrl Pts',(-38.7181664204435,-27.6739897756341,1.05512748361982));
#7169=CARTESIAN_POINT('Ctrl Pts',(-39.537436538438,-27.5211153732406,1.10805572336171));
#7170=CARTESIAN_POINT('Ctrl Pts',(-40.3567066564326,-27.368240970847,1.16098396310361));
#7171=CARTESIAN_POINT('Ctrl Pts',(-41.2592565451631,-27.6616899420598,1.2139122028455));
#7172=CARTESIAN_POINT('Ctrl Pts',(-41.8319594110142,-28.2671482889205,1.26684044258739));
#7173=CARTESIAN_POINT('Ctrl Pts',(-42.2668524352508,-28.7269148226958,1.30703252756093));
#7174=CARTESIAN_POINT('Ctrl Pts',(-42.5115418566941,-29.3665990250785,1.34722461253447));
#7175=CARTESIAN_POINT('Ctrl Pts',(-42.517348422246,-30.0023034643409,1.38741669750801));
#7176=CARTESIAN_POINT('Origin',(-40.,-30.,5.));
#7177=CARTESIAN_POINT('',(-42.5213132441747,-29.9991346486057,2.38741669750801));
#7178=CARTESIAN_POINT('',(-42.5158084819528,-29.9978709045252,2.11258330249198));
#7179=CARTESIAN_POINT('',(-42.5175,-30.,5.));
#7180=CARTESIAN_POINT('Ctrl Pts',(-42.5158084819528,-29.9978709045252,2.11258330249198));
#7181=CARTESIAN_POINT('Ctrl Pts',(-42.5178587672328,-29.7423941346425,2.09645598497262));
#7182=CARTESIAN_POINT('Ctrl Pts',(-42.4820672379611,-29.4874783703648,2.08032866745326));
#7183=CARTESIAN_POINT('Ctrl Pts',(-42.4060544530648,-29.2451807415716,2.06420134993389));
#7184=CARTESIAN_POINT('Ctrl Pts',(-42.1565881113989,-28.4499842080957,2.011273110192));
#7185=CARTESIAN_POINT('Ctrl Pts',(-41.4739040096323,-27.7906959227911,1.9583448704501));
#7186=CARTESIAN_POINT('Ctrl Pts',(-40.6704950327292,-27.5690980688551,1.90541663070821));
#7187=CARTESIAN_POINT('Ctrl Pts',(-39.867086055826,-27.3475002149192,1.85248839096631));
#7188=CARTESIAN_POINT('Ctrl Pts',(-38.9429522037861,-27.5635927923519,1.79956015122442));
#7189=CARTESIAN_POINT('Ctrl Pts',(-38.321108361921,-28.1184643721705,1.74663191148252));
#7190=CARTESIAN_POINT('Ctrl Pts',(-37.6992645200558,-28.673335951989,1.69370367174063));
#7191=CARTESIAN_POINT('Ctrl Pts',(-37.3797106883653,-29.5669865341932,1.64077543199874));
#7192=CARTESIAN_POINT('Ctrl Pts',(-37.508719499589,-30.3903486277475,1.58784719225684));
#7193=CARTESIAN_POINT('Ctrl Pts',(-37.6377283108126,-31.2137107213018,1.53491895251495));
#7194=CARTESIAN_POINT('Ctrl Pts',(-38.2152997649503,-31.9667843262062,1.48199071277305));
#7195=CARTESIAN_POINT('Ctrl Pts',(-38.9770562866683,-32.3048688388086,1.42906247303116));
#7196=CARTESIAN_POINT('Ctrl Pts',(-39.7388128083864,-32.642953351411,1.37613423328926));
#7197=CARTESIAN_POINT('Ctrl Pts',(-40.6847543976847,-32.5660487717114,1.32320599354737));
#7198=CARTESIAN_POINT('Ctrl Pts',(-41.3818821333116,-32.1093323330538,1.27027775380548));
#7199=CARTESIAN_POINT('Ctrl Pts',(-42.0742231614735,-31.6557518591192,1.21771293670098));
#7200=CARTESIAN_POINT('Ctrl Pts',(-42.521155480172,-30.8275574448016,1.16514811959648));
#7201=CARTESIAN_POINT('Ctrl Pts',(-42.5216691698492,-29.9998787127942,1.11258330249199));
#7202=CARTESIAN_POINT('Ctrl Pts',(-42.517348422246,-30.0023034643409,1.38741669750801));
#7203=CARTESIAN_POINT('Ctrl Pts',(-42.5191884192899,-30.2037468612362,1.40015285227637));
#7204=CARTESIAN_POINT('Ctrl Pts',(-42.4970411605304,-30.4047906329863,1.41288900704472));
#7205=CARTESIAN_POINT('Ctrl Pts',(-42.4493576963842,-30.5995832549246,1.42562516181308));
#7206=CARTESIAN_POINT('Ctrl Pts',(-42.2511972729315,-31.4090921515597,1.47855340155497));
#7207=CARTESIAN_POINT('Ctrl Pts',(-41.6120205830545,-32.1106422223213,1.53148164129687));
#7208=CARTESIAN_POINT('Ctrl Pts',(-40.8244074737101,-32.3831071850833,1.58440988103876));
#7209=CARTESIAN_POINT('Ctrl Pts',(-40.0367943643657,-32.6555721478454,1.63733812078065));
#7210=CARTESIAN_POINT('Ctrl Pts',(-39.100744835554,-32.4989520026077,1.69026636052255));
#7211=CARTESIAN_POINT('Ctrl Pts',(-38.4447268280219,-31.9849370913482,1.74319460026444));
#7212=CARTESIAN_POINT('Ctrl Pts',(-37.7887088204899,-31.4709221800887,1.79612284000634));
#7213=CARTESIAN_POINT('Ctrl Pts',(-37.4127223342376,-30.5995125028073,1.84905107974823));
#7214=CARTESIAN_POINT('Ctrl Pts',(-37.4888725784047,-29.7695892606159,1.90197931949013));
#7215=CARTESIAN_POINT('Ctrl Pts',(-37.5650228225718,-28.9396660184245,1.95490755923202));
#7216=CARTESIAN_POINT('Ctrl Pts',(-38.0933097971584,-28.1512292113232,2.00783579897392));
#7217=CARTESIAN_POINT('Ctrl Pts',(-38.8319142523488,-27.7651789657407,2.06076403871581));
#7218=CARTESIAN_POINT('Ctrl Pts',(-39.5705187075392,-27.3791287201582,2.11369227845771));
#7219=CARTESIAN_POINT('Ctrl Pts',(-40.5194406433335,-27.3954650360944,2.1666205181996));
#7220=CARTESIAN_POINT('Ctrl Pts',(-41.2443190068267,-27.8067102550096,2.2195487579415));
#7221=CARTESIAN_POINT('Ctrl Pts',(-41.96919737032,-28.2179554739248,2.27247699768339));
#7222=CARTESIAN_POINT('Ctrl Pts',(-42.4700321615123,-29.0241095958189,2.32540523742529));
#7223=CARTESIAN_POINT('Ctrl Pts',(-42.5175703285892,-29.8561621522147,2.37833347716718));
#7224=CARTESIAN_POINT('Ctrl Pts',(-42.5202897316166,-29.9037594067979,2.38136121728079));
#7225=CARTESIAN_POINT('Ctrl Pts',(-42.5215257807612,-29.9514414106188,2.3843889573944));
#7226=CARTESIAN_POINT('Ctrl Pts',(-42.5213132441747,-29.9991346486057,2.38741669750801));
#7227=CARTESIAN_POINT('Origin',(-40.,-30.,5.));
#7228=CARTESIAN_POINT('',(-42.5147867566421,-29.9982362786167,3.38741669750801));
#7229=CARTESIAN_POINT('',(-42.5141172985733,-30.0013301677674,3.11258330249199));
#7230=CARTESIAN_POINT('',(-42.5175,-30.,5.));
#7231=CARTESIAN_POINT('Ctrl Pts',(-42.5141172985733,-30.0013301677674,3.11258330249199));
#7232=CARTESIAN_POINT('Ctrl Pts',(-42.5116926131382,-29.4952784299888,3.08069209009066));
#7233=CARTESIAN_POINT('Ctrl Pts',(-42.3636224339317,-28.9879212311263,3.04880087768933));
#7234=CARTESIAN_POINT('Ctrl Pts',(-42.0796113410677,-28.5737929421548,3.01690966528799));
#7235=CARTESIAN_POINT('Ctrl Pts',(-41.608252428045,-27.8864850691663,2.9639814255461));
#7236=CARTESIAN_POINT('Ctrl Pts',(-40.762452834543,-27.4559703537395,2.9110531858042));
#7237=CARTESIAN_POINT('Ctrl Pts',(-39.9293703365743,-27.4793133260285,2.85812494606231));
#7238=CARTESIAN_POINT('Ctrl Pts',(-39.0962878386057,-27.5026562983174,2.80519670632041));
#7239=CARTESIAN_POINT('Ctrl Pts',(-38.2759224361703,-27.979856958322,2.75226846657852));
#7240=CARTESIAN_POINT('Ctrl Pts',(-37.8437896202483,-28.6924806952517,2.69934022683663));
#7241=CARTESIAN_POINT('Ctrl Pts',(-37.4116568043264,-29.4051044321814,2.64641198709473));
#7242=CARTESIAN_POINT('Ctrl Pts',(-37.3677565749178,-30.3531512460361,2.59348374735284));
#7243=CARTESIAN_POINT('Ctrl Pts',(-37.7321838916479,-31.1026604387066,2.54055550761094));
#7244=CARTESIAN_POINT('Ctrl Pts',(-38.0966112083779,-31.8521696313771,2.48762726786905));
#7245=CARTESIAN_POINT('Ctrl Pts',(-38.8693660712466,-32.4031412028634,2.43469902812715));
#7246=CARTESIAN_POINT('Ctrl Pts',(-39.6967263399719,-32.5033726659385,2.38177078838526));
#7247=CARTESIAN_POINT('Ctrl Pts',(-40.5240866086972,-32.6036041290136,2.32884254864336));
#7248=CARTESIAN_POINT('Ctrl Pts',(-41.4060522832791,-32.2530954836775,2.27591430890147));
#7249=CARTESIAN_POINT('Ctrl Pts',(-41.9389108297875,-31.612288770186,2.22298606915957));
#7250=CARTESIAN_POINT('Ctrl Pts',(-42.3094065428755,-31.1667368656095,2.18618514693704));
#7251=CARTESIAN_POINT('Ctrl Pts',(-42.5111299364331,-30.5808432882975,2.14938422471451));
#7252=CARTESIAN_POINT('Ctrl Pts',(-42.5158084819528,-29.9978709045252,2.11258330249198));
#7253=CARTESIAN_POINT('Ctrl Pts',(-42.5213132441747,-29.9991346486057,2.38741669750801));
#7254=CARTESIAN_POINT('Ctrl Pts',(-42.5178104065942,-30.7851718628753,2.43731719713629));
#7255=CARTESIAN_POINT('Ctrl Pts',(-42.1208328792847,-31.5742605775652,2.48721769676458));
#7256=CARTESIAN_POINT('Ctrl Pts',(-41.4860275712473,-32.0372951840482,2.53711819639286));
#7257=CARTESIAN_POINT('Ctrl Pts',(-40.8127051038668,-32.5284246685882,2.59004643613476));
#7258=CARTESIAN_POINT('Ctrl Pts',(-39.8718186261444,-32.6527326467706,2.64297467587665));
#7259=CARTESIAN_POINT('Ctrl Pts',(-39.0940511361637,-32.3533181488389,2.69590291561855));
#7260=CARTESIAN_POINT('Ctrl Pts',(-38.3162836461829,-32.0539036509073,2.74883115536044));
#7261=CARTESIAN_POINT('Ctrl Pts',(-37.7016351439439,-31.3307666768615,2.80175939510233));
#7262=CARTESIAN_POINT('Ctrl Pts',(-37.5314559124885,-30.5149172135064,2.85468763484423));
#7263=CARTESIAN_POINT('Ctrl Pts',(-37.361276681033,-29.6990677501512,2.90761587458612));
#7264=CARTESIAN_POINT('Ctrl Pts',(-37.6355667203612,-28.7905057974866,2.96054411432802));
#7265=CARTESIAN_POINT('Ctrl Pts',(-38.2287720265447,-28.2051180801097,3.01347235406991));
#7266=CARTESIAN_POINT('Ctrl Pts',(-38.8219773327282,-27.6197303627328,3.06640059381181));
#7267=CARTESIAN_POINT('Ctrl Pts',(-39.7340979057671,-27.3575168806436,3.1193288335537));
#7268=CARTESIAN_POINT('Ctrl Pts',(-40.5476180890752,-27.5385036919369,3.1722570732956));
#7269=CARTESIAN_POINT('Ctrl Pts',(-41.3611382723834,-27.7194905032302,3.22518531303749));
#7270=CARTESIAN_POINT('Ctrl Pts',(-42.0760580659608,-28.3436776079059,3.27811355277939));
#7271=CARTESIAN_POINT('Ctrl Pts',(-42.3651288382537,-29.1253485131059,3.33104179252128));
#7272=CARTESIAN_POINT('Ctrl Pts',(-42.4677604856938,-29.4028728443289,3.34983342751686));
#7273=CARTESIAN_POINT('Ctrl Pts',(-42.5167124568098,-29.7002485290033,3.36862506251243));
#7274=CARTESIAN_POINT('Ctrl Pts',(-42.5147867566421,-29.9982362786167,3.38741669750801));
#7275=CARTESIAN_POINT('Origin',(-40.,-30.,5.));
#7276=CARTESIAN_POINT('',(-42.5149325414735,-30.0018328375922,4.38741669750801));
#7277=CARTESIAN_POINT('',(-42.5206616850174,-30.0014234824409,4.11258330249199));
#7278=CARTESIAN_POINT('',(-42.5175,-30.,5.));
#7279=CARTESIAN_POINT('Ctrl Pts',(-42.5206616850174,-30.0014234824409,4.11258330249199));
#7280=CARTESIAN_POINT('Ctrl Pts',(-42.5155795866941,-29.2502422402753,4.06492819520869));
#7281=CARTESIAN_POINT('Ctrl Pts',(-42.1578863186577,-28.4948606212539,4.01727308792539));
#7282=CARTESIAN_POINT('Ctrl Pts',(-41.5708988488514,-28.0274060986095,3.9696179806421));
#7283=CARTESIAN_POINT('Ctrl Pts',(-40.9189600473564,-27.5082268027603,3.9166897409002));
#7284=CARTESIAN_POINT('Ctrl Pts',(-39.9841758778376,-27.3442193556112,3.8637615011583));
#7285=CARTESIAN_POINT('Ctrl Pts',(-39.1944360729249,-27.6104568110664,3.81083326141641));
#7286=CARTESIAN_POINT('Ctrl Pts',(-38.4046962680121,-27.8766942665217,3.75790502167452));
#7287=CARTESIAN_POINT('Ctrl Pts',(-37.7600008277053,-28.5731766245815,3.70497678193262));
#7288=CARTESIAN_POINT('Ctrl Pts',(-37.5554537649444,-29.38109483929,3.65204854219073));
#7289=CARTESIAN_POINT('Ctrl Pts',(-37.3509067021835,-30.1890130539986,3.59912030244883));
#7290=CARTESIAN_POINT('Ctrl Pts',(-37.5865080169685,-31.1083671253559,3.54619206270694));
#7291=CARTESIAN_POINT('Ctrl Pts',(-38.1544131533048,-31.7183303191202,3.49326382296504));
#7292=CARTESIAN_POINT('Ctrl Pts',(-38.7223182896412,-32.3282935128845,3.44033558322315));
#7293=CARTESIAN_POINT('Ctrl Pts',(-39.6225272475288,-32.6288658290557,3.38740734348126));
#7294=CARTESIAN_POINT('Ctrl Pts',(-40.4429768120994,-32.4824627756441,3.33447910373936));
#7295=CARTESIAN_POINT('Ctrl Pts',(-41.26342637667,-32.3360597222325,3.28155086399747));
#7296=CARTESIAN_POINT('Ctrl Pts',(-42.0041165479235,-31.742681299238,3.22862262425557));
#7297=CARTESIAN_POINT('Ctrl Pts',(-42.3260025172786,-30.9739415724657,3.17569438451368));
#7298=CARTESIAN_POINT('Ctrl Pts',(-42.4539403434918,-30.6683958235659,3.15465735717311));
#7299=CARTESIAN_POINT('Ctrl Pts',(-42.5157167414903,-30.3351470233143,3.13362032983255));
#7300=CARTESIAN_POINT('Ctrl Pts',(-42.5141172985733,-30.0013301677674,3.11258330249199));
#7301=CARTESIAN_POINT('Ctrl Pts',(-42.5147867566421,-29.9982362786167,3.38741669750801));
#7302=CARTESIAN_POINT('Ctrl Pts',(-42.511288558348,-30.5395563941995,3.42155330225433));
#7303=CARTESIAN_POINT('Ctrl Pts',(-42.339894983855,-31.0828963127842,3.45568990700064));
#7304=CARTESIAN_POINT('Ctrl Pts',(-42.0174032055179,-31.5129223213822,3.48982651174696));
#7305=CARTESIAN_POINT('Ctrl Pts',(-41.5173850494808,-32.1796705187342,3.54275475148886));
#7306=CARTESIAN_POINT('Ctrl Pts',(-40.6541269863983,-32.5740122077138,3.59568299123075));
#7307=CARTESIAN_POINT('Ctrl Pts',(-39.8227782642378,-32.5154407369856,3.64861123097265));
#7308=CARTESIAN_POINT('Ctrl Pts',(-38.9914295420773,-32.4568692662574,3.70153947071454));
#7309=CARTESIAN_POINT('Ctrl Pts',(-38.1919901608389,-31.9453846358214,3.75446771045644));
#7310=CARTESIAN_POINT('Ctrl Pts',(-37.7903968943648,-31.2151147107584,3.80739595019833));
#7311=CARTESIAN_POINT('Ctrl Pts',(-37.3888036278907,-30.4848447856954,3.86032418994022));
#7312=CARTESIAN_POINT('Ctrl Pts',(-37.3850564761809,-29.5357895660055,3.91325242968212));
#7313=CARTESIAN_POINT('Ctrl Pts',(-37.7808706669184,-28.8023712396148,3.96618066942401));
#7314=CARTESIAN_POINT('Ctrl Pts',(-38.1766848576559,-28.0689529132242,4.01910890916591));
#7315=CARTESIAN_POINT('Ctrl Pts',(-38.9720603908406,-27.5511714801328,4.0720371489078));
#7316=CARTESIAN_POINT('Ctrl Pts',(-39.8029206856667,-27.486037114713,4.1249653886497));
#7317=CARTESIAN_POINT('Ctrl Pts',(-40.6337809804928,-27.4209027492932,4.17789362839159));
#7318=CARTESIAN_POINT('Ctrl Pts',(-41.5001260369602,-27.8084154515449,4.23082186813349));
#7319=CARTESIAN_POINT('Ctrl Pts',(-42.005393561113,-28.4711944826902,4.28375010787538));
#7320=CARTESIAN_POINT('Ctrl Pts',(-42.3352701470746,-28.9039064097189,4.31830563775292));
#7321=CARTESIAN_POINT('Ctrl Pts',(-42.5112389161138,-29.45394948023,4.35286116763047));
#7322=CARTESIAN_POINT('Ctrl Pts',(-42.5149325414735,-30.0018328375922,4.38741669750801));
#7323=CARTESIAN_POINT('Origin',(-40.,-30.,5.));
#7324=CARTESIAN_POINT('',(-42.521402710782,-30.0007512051302,5.38741669750801));
#7325=CARTESIAN_POINT('',(-42.5184257094164,-29.9977798166958,5.11258330249199));
#7326=CARTESIAN_POINT('',(-42.5175,-30.,5.));
#7327=CARTESIAN_POINT('Ctrl Pts',(-42.5184257094164,-29.9977798166958,5.11258330249199));
#7328=CARTESIAN_POINT('Ctrl Pts',(-42.5199490958157,-29.8320331685022,5.10209254006862));
#7329=CARTESIAN_POINT('Ctrl Pts',(-42.50498599437,-29.666560233277,5.09160177764525));
#7330=CARTESIAN_POINT('Ctrl Pts',(-42.4725332000196,-29.504591615208,5.08111101522188));
#7331=CARTESIAN_POINT('Ctrl Pts',(-42.3088016035587,-28.6874237582064,5.02818277547999));
#7332=CARTESIAN_POINT('Ctrl Pts',(-41.6998824869394,-27.9594557672715,4.97525453573809));
#7333=CARTESIAN_POINT('Ctrl Pts',(-40.9245035463699,-27.6539089775381,4.9223262959962));
#7334=CARTESIAN_POINT('Ctrl Pts',(-40.1491246058004,-27.3483621878047,4.8693980562543));
#7335=CARTESIAN_POINT('Ctrl Pts',(-39.2072858412808,-27.4652365992728,4.81646981651241));
#7336=CARTESIAN_POINT('Ctrl Pts',(-38.5301061680647,-27.9510339154214,4.76354157677051));
#7337=CARTESIAN_POINT('Ctrl Pts',(-37.8529264948486,-28.4368312315701,4.71061333702862));
#7338=CARTESIAN_POINT('Ctrl Pts',(-37.440405912936,-29.2915514523993,4.65768509728673));
#7339=CARTESIAN_POINT('Ctrl Pts',(-37.4813723114462,-30.1239534564781,4.60475685754483));
#7340=CARTESIAN_POINT('Ctrl Pts',(-37.5223387099564,-30.956355460557,4.55182861780294));
#7341=CARTESIAN_POINT('Ctrl Pts',(-38.0167920888894,-31.7664392478856,4.49890037806104));
#7342=CARTESIAN_POINT('Ctrl Pts',(-38.7384004980203,-32.1833956557518,4.44597213831915));
#7343=CARTESIAN_POINT('Ctrl Pts',(-39.4600089071513,-32.600352063618,4.39304389857725));
#7344=CARTESIAN_POINT('Ctrl Pts',(-40.4087723464802,-32.6241810920218,4.34011565883536));
#7345=CARTESIAN_POINT('Ctrl Pts',(-41.1504021880581,-32.2439752000789,4.28718741909346));
#7346=CARTESIAN_POINT('Ctrl Pts',(-41.8920320296359,-31.863769308136,4.23425917935157));
#7347=CARTESIAN_POINT('Ctrl Pts',(-42.4265282734626,-31.0795284958463,4.18133093960967));
#7348=CARTESIAN_POINT('Ctrl Pts',(-42.5092296786403,-30.250232517427,4.12840269986778));
#7349=CARTESIAN_POINT('Ctrl Pts',(-42.5174690507815,-30.1676114523224,4.12312956740918));
#7350=CARTESIAN_POINT('Ctrl Pts',(-42.5212240293106,-30.0845431818009,4.11785643495058));
#7351=CARTESIAN_POINT('Ctrl Pts',(-42.5206616850174,-30.0014234824409,4.11258330249199));
#7352=CARTESIAN_POINT('Ctrl Pts',(-42.5149325414735,-30.0018328375922,4.38741669750801));
#7353=CARTESIAN_POINT('Ctrl Pts',(-42.516896392334,-30.2931350401628,4.40578940737236));
#7354=CARTESIAN_POINT('Ctrl Pts',(-42.4701596848035,-30.5838267121945,4.42416211723671));
#7355=CARTESIAN_POINT('Ctrl Pts',(-42.3719617588218,-30.8559480471321,4.44253482710106));
#7356=CARTESIAN_POINT('Ctrl Pts',(-42.0890724405397,-31.6398772203896,4.49546306684296));
#7357=CARTESIAN_POINT('Ctrl Pts',(-41.3791038121377,-32.2696902068656,4.54839130658486));
#7358=CARTESIAN_POINT('Ctrl Pts',(-40.5670381492107,-32.4570953139945,4.60131954632675));
#7359=CARTESIAN_POINT('Ctrl Pts',(-39.7549724862838,-32.6445004211234,4.65424778606864));
#7360=CARTESIAN_POINT('Ctrl Pts',(-38.840809788832,-32.3894976489052,4.70717602581054));
#7361=CARTESIAN_POINT('Ctrl Pts',(-38.243000481004,-31.8088124101068,4.76010426555243));
#7362=CARTESIAN_POINT('Ctrl Pts',(-37.645191173176,-31.2281271713084,4.81303250529432));
#7363=CARTESIAN_POINT('Ctrl Pts',(-37.3637352549718,-30.3217594659298,4.86596074503622));
#7364=CARTESIAN_POINT('Ctrl Pts',(-37.5274668482371,-29.504591624877,4.91888898477811));
#7365=CARTESIAN_POINT('Ctrl Pts',(-37.6911984415025,-28.6874237838241,4.97181722452001));
#7366=CARTESIAN_POINT('Ctrl Pts',(-38.3001175462374,-27.959455807097,5.0247454642619));
#7367=CARTESIAN_POINT('Ctrl Pts',(-39.0754964716737,-27.653909023327,5.0776737040038));
#7368=CARTESIAN_POINT('Ctrl Pts',(-39.85087539711,-27.348362239557,5.1306019437457));
#7369=CARTESIAN_POINT('Ctrl Pts',(-40.7927141432477,-27.465236648744,5.18353018348759));
#7370=CARTESIAN_POINT('Ctrl Pts',(-41.4698938032473,-27.9510339554113,5.23645842322948));
#7371=CARTESIAN_POINT('Ctrl Pts',(-42.1136955075206,-28.4128864776267,5.28677784798899));
#7372=CARTESIAN_POINT('Ctrl Pts',(-42.5182850573256,-29.2081900157384,5.3370972727485));
#7373=CARTESIAN_POINT('Ctrl Pts',(-42.521402710782,-30.0007512051302,5.38741669750801));
#7374=CARTESIAN_POINT('Origin',(-40.,-30.,5.));
#7375=CARTESIAN_POINT('',(-42.5171494503087,-29.9976988316789,6.38741669750801));
#7376=CARTESIAN_POINT('',(-42.5134147285392,-29.9999453848359,6.11258330249199));
#7377=CARTESIAN_POINT('',(-42.5175,-30.,5.));
#7378=CARTESIAN_POINT('Ctrl Pts',(-42.5134147285392,-29.9999453848359,6.11258330249199));
#7379=CARTESIAN_POINT('Ctrl Pts',(-42.5134953811471,-29.5830437993479,6.08632864518665));
#7380=CARTESIAN_POINT('Ctrl Pts',(-42.4154700479868,-29.1661778965789,6.06007398788132));
#7381=CARTESIAN_POINT('Ctrl Pts',(-42.2191293763926,-28.8023712162405,6.03381933057598));
#7382=CARTESIAN_POINT('Ctrl Pts',(-41.82331517793,-28.0689528755357,5.98089109083409));
#7383=CARTESIAN_POINT('Ctrl Pts',(-41.0279396292218,-27.5511714323388,5.92796285109219));
#7384=CARTESIAN_POINT('Ctrl Pts',(-40.1970793181797,-27.4860370656477,5.8750346113503));
#7385=CARTESIAN_POINT('Ctrl Pts',(-39.3662190071376,-27.4209026989567,5.8221063716084));
#7386=CARTESIAN_POINT('Ctrl Pts',(-38.4998739337617,-27.8084154087715,5.76917813186651));
#7387=CARTESIAN_POINT('Ctrl Pts',(-37.9946063997475,-28.4711944528524,5.71624989212461));
#7388=CARTESIAN_POINT('Ctrl Pts',(-37.4893388657334,-29.1339734969332,5.66332165238272));
#7389=CARTESIAN_POINT('Ctrl Pts',(-37.3451488710812,-30.0720188752802,5.61039341264082));
#7390=CARTESIAN_POINT('Ctrl Pts',(-37.6280381948844,-30.8559480638377,5.55746517289893));
#7391=CARTESIAN_POINT('Ctrl Pts',(-37.9109275186876,-31.6398772523952,5.50453693315704));
#7392=CARTESIAN_POINT('Ctrl Pts',(-38.6208961609462,-32.2696902511634,5.45160869341514));
#7393=CARTESIAN_POINT('Ctrl Pts',(-39.4329618397223,-32.4570953619499,5.39868045367325));
#7394=CARTESIAN_POINT('Ctrl Pts',(-40.2450275184985,-32.6445004727364,5.34575221393135));
#7395=CARTESIAN_POINT('Ctrl Pts',(-41.1591902337921,-32.3894976955413,5.29282397418946));
#7396=CARTESIAN_POINT('Ctrl Pts',(-41.7569995532876,-31.8088124454096,5.23989573444756));
#7397=CARTESIAN_POINT('Ctrl Pts',(-42.2363187137321,-31.3432232391213,5.19745825712904));
#7398=CARTESIAN_POINT('Ctrl Pts',(-42.5122632711536,-30.6682620313788,5.15502077981051));
#7399=CARTESIAN_POINT('Ctrl Pts',(-42.5184257094164,-29.9977798166958,5.11258330249199));
#7400=CARTESIAN_POINT('Ctrl Pts',(-42.521402710782,-30.0007512051302,5.38741669750801));
#7401=CARTESIAN_POINT('Ctrl Pts',(-42.5215643457984,-30.041841609387,5.39002551249039));
#7402=CARTESIAN_POINT('Ctrl Pts',(-42.5206468592439,-30.0829246424488,5.39263432747278));
#7403=CARTESIAN_POINT('Ctrl Pts',(-42.5186276393975,-30.1239534540589,5.39524314245516));
#7404=CARTESIAN_POINT('Ctrl Pts',(-42.4776612416868,-30.9563554418917,5.44817138219706));
#7405=CARTESIAN_POINT('Ctrl Pts',(-41.9832078724042,-31.7664392134098,5.50109962193896));
#7406=CARTESIAN_POINT('Ctrl Pts',(-41.2615994773569,-32.1833956131383,5.55402786168085));
#7407=CARTESIAN_POINT('Ctrl Pts',(-40.5399910823097,-32.6003520128667,5.60695610142275));
#7408=CARTESIAN_POINT('Ctrl Pts',(-39.5912276614978,-32.6241810408054,5.65988434116464));
#7409=CARTESIAN_POINT('Ctrl Pts',(-38.8495978343945,-32.243975156283,5.71281258090653));
#7410=CARTESIAN_POINT('Ctrl Pts',(-38.1079680072911,-31.8637692717606,5.76574082064843));
#7411=CARTESIAN_POINT('Ctrl Pts',(-37.5734717738962,-31.0795284747771,5.81866906039032));
#7412=CARTESIAN_POINT('Ctrl Pts',(-37.4907703703327,-30.2502325125432,5.87159730013222));
#7413=CARTESIAN_POINT('Ctrl Pts',(-37.4080689667691,-29.4209365503093,5.92452553987411));
#7414=CARTESIAN_POINT('Ctrl Pts',(-37.7771623930368,-28.546585422825,5.97745377961601));
#7415=CARTESIAN_POINT('Ctrl Pts',(-38.429101181808,-28.0274061371088,6.0303820193579));
#7416=CARTESIAN_POINT('Ctrl Pts',(-39.0810399705791,-27.5082268513926,6.08331025909979));
#7417=CARTESIAN_POINT('Ctrl Pts',(-40.0158241218535,-27.3442194074445,6.13623849884169));
#7418=CARTESIAN_POINT('Ctrl Pts',(-40.8055639113529,-27.6104568577035,6.18916673858358));
#7419=CARTESIAN_POINT('Ctrl Pts',(-41.5953037008522,-27.8766943079625,6.24209497832548));
#7420=CARTESIAN_POINT('Ctrl Pts',(-42.2399991285764,-28.5731766524286,6.29502321806738));
#7421=CARTESIAN_POINT('Ctrl Pts',(-42.4445461873451,-29.3810948513691,6.34795145780927));
#7422=CARTESIAN_POINT('Ctrl Pts',(-42.495385454142,-29.5818993464971,6.36110653770885));
#7423=CARTESIAN_POINT('Ctrl Pts',(-42.5190345977134,-29.7895877808343,6.37426161760843));
#7424=CARTESIAN_POINT('Ctrl Pts',(-42.5171494503087,-29.9976988316789,6.38741669750801));
#7425=CARTESIAN_POINT('Origin',(-40.,-30.,5.));
#7426=CARTESIAN_POINT('',(-42.5135602932616,-30.0006322084125,7.38741669750801));
#7427=CARTESIAN_POINT('',(-42.5182251666708,-30.0022480740648,7.11258330249199));
#7428=CARTESIAN_POINT('',(-42.5175,-30.,5.));
#7429=CARTESIAN_POINT('Ctrl Pts',(-42.5182251666708,-30.0022480740648,7.11258330249199));
#7430=CARTESIAN_POINT('Ctrl Pts',(-42.5120992560187,-29.3382485831854,7.07056475030469));
#7431=CARTESIAN_POINT('Ctrl Pts',(-42.2421605144463,-28.6698443415211,7.02854619811738));
#7432=CARTESIAN_POINT('Ctrl Pts',(-41.771228008025,-28.2051180450781,6.98652764593008));
#7433=CARTESIAN_POINT('Ctrl Pts',(-41.1780226902642,-27.6197303162755,6.93359940618819));
#7434=CARTESIAN_POINT('Ctrl Pts',(-40.2659020994226,-27.35751682907,6.88067116644629));
#7435=CARTESIAN_POINT('Ctrl Pts',(-39.4523819002367,-27.538503643896,6.8277429267044));
#7436=CARTESIAN_POINT('Ctrl Pts',(-38.6388617010508,-27.7194904587219,6.77481468696251));
#7437=CARTESIAN_POINT('Ctrl Pts',(-37.9239418935206,-28.3436775755792,6.72188644722061));
#7438=CARTESIAN_POINT('Ctrl Pts',(-37.6348711155859,-29.125348496035,6.66895820747872));
#7439=CARTESIAN_POINT('Ctrl Pts',(-37.3458003376513,-29.9070194164908,6.61602996773682));
#7440=CARTESIAN_POINT('Ctrl Pts',(-37.4825785893123,-30.8461741405451,6.56310172799493));
#7441=CARTESIAN_POINT('Ctrl Pts',(-37.9825967551082,-31.5129223509102,6.51017348825303));
#7442=CARTESIAN_POINT('Ctrl Pts',(-38.4826149209041,-32.1796705612752,6.45724524851114));
#7443=CARTESIAN_POINT('Ctrl Pts',(-39.345873000835,-32.5740122579511,6.40431700876924));
#7444=CARTESIAN_POINT('Ctrl Pts',(-40.1772217392211,-32.5154407860797,6.35138876902735));
#7445=CARTESIAN_POINT('Ctrl Pts',(-41.0085704776071,-32.4568693142083,6.29846052928545));
#7446=CARTESIAN_POINT('Ctrl Pts',(-41.8080098744483,-31.9453846737896,6.24553228954356));
#7447=CARTESIAN_POINT('Ctrl Pts',(-42.2096031487603,-31.2151147344739,6.19260404980166));
#7448=CARTESIAN_POINT('Ctrl Pts',(-42.4119890841431,-30.8470897345444,6.16593046736511));
#7449=CARTESIAN_POINT('Ctrl Pts',(-42.5133327890205,-30.4234991444269,6.13925688492855));
#7450=CARTESIAN_POINT('Ctrl Pts',(-42.5134147285392,-29.9999453848359,6.11258330249199));
#7451=CARTESIAN_POINT('Ctrl Pts',(-42.5171494503087,-29.9976988316789,6.38741669750801));
#7452=CARTESIAN_POINT('Ctrl Pts',(-42.5114498825654,-30.6269032267395,6.42718985735033));
#7453=CARTESIAN_POINT('Ctrl Pts',(-42.2723416287469,-31.2599707548622,6.46696301719264));
#7454=CARTESIAN_POINT('Ctrl Pts',(-41.8455868106747,-31.7183302855837,6.50673617703495));
#7455=CARTESIAN_POINT('Ctrl Pts',(-41.2776816854222,-32.3282934674429,6.55966441677685));
#7456=CARTESIAN_POINT('Ctrl Pts',(-40.3774727451039,-32.6288657777464,6.61259265651874));
#7457=CARTESIAN_POINT('Ctrl Pts',(-39.5570231965462,-32.4824627271928,6.66552089626064));
#7458=CARTESIAN_POINT('Ctrl Pts',(-38.7365736479884,-32.3360596766392,6.71844913600253));
#7459=CARTESIAN_POINT('Ctrl Pts',(-37.9958834911912,-31.7426812652287,6.77137737574443));
#7460=CARTESIAN_POINT('Ctrl Pts',(-37.6739975281183,-30.9739415534587,6.82430561548632));
#7461=CARTESIAN_POINT('Ctrl Pts',(-37.3521115650454,-30.2052018416886,6.87723385522821));
#7462=CARTESIAN_POINT('Ctrl Pts',(-37.4490297956967,-29.261100829559,6.9301620949701));
#7463=CARTESIAN_POINT('Ctrl Pts',(-37.9203886995201,-28.5737929699874,6.983090334712));
#7464=CARTESIAN_POINT('Ctrl Pts',(-38.3917476033435,-27.8864851104157,7.0360185744539));
#7465=CARTESIAN_POINT('Ctrl Pts',(-39.237547180339,-27.4559704034018,7.08894681419579));
#7466=CARTESIAN_POINT('Ctrl Pts',(-40.0706296620477,-27.4793133752305,7.14187505393769));
#7467=CARTESIAN_POINT('Ctrl Pts',(-40.9037121437564,-27.5026563470591,7.19480329367958));
#7468=CARTESIAN_POINT('Ctrl Pts',(-41.7240775301785,-27.9798569977301,7.24773153342147));
#7469=CARTESIAN_POINT('Ctrl Pts',(-42.1562103376676,-28.6924807207603,7.30065977316337));
#7470=CARTESIAN_POINT('Ctrl Pts',(-42.392319413333,-29.0818446515379,7.32957874794491));
#7471=CARTESIAN_POINT('Ctrl Pts',(-42.5125286425665,-29.5414899018482,7.35849772272646));
#7472=CARTESIAN_POINT('Ctrl Pts',(-42.5135602932616,-30.0006322084125,7.38741669750801));
#7473=CARTESIAN_POINT('Origin',(-40.,-30.,5.));
#7474=CARTESIAN_POINT('',(-42.51946795121,-30.0019779683886,8.38741669750802));
#7475=CARTESIAN_POINT('',(-42.5208030005754,-29.9986726513939,8.11258330249199));
#7476=CARTESIAN_POINT('',(-42.5175,-30.,5.));
#7477=CARTESIAN_POINT('Ctrl Pts',(-42.5208030005754,-29.9986726513939,8.11258330249199));
#7478=CARTESIAN_POINT('Ctrl Pts',(-42.5212923589469,-29.922167703349,8.10772909516461));
#7479=CARTESIAN_POINT('Ctrl Pts',(-42.5181114375889,-29.8457040028919,8.10287488783724));
#7480=CARTESIAN_POINT('Ctrl Pts',(-42.5111274705733,-29.7695892561818,8.09802068050987));
#7481=CARTESIAN_POINT('Ctrl Pts',(-42.4349772248954,-28.9396659978463,8.04509244076797));
#7482=CARTESIAN_POINT('Ctrl Pts',(-41.9066902400584,-28.151229175236,7.99216420102608));
#7483=CARTESIAN_POINT('Ctrl Pts',(-41.1680857704662,-27.7651789220903,7.93923596128419));
#7484=CARTESIAN_POINT('Ctrl Pts',(-40.4294813008741,-27.3791286689446,7.88630772154229));
#7485=CARTESIAN_POINT('Ctrl Pts',(-39.4805593465267,-27.3954649852637,7.83337948180039));
#7486=CARTESIAN_POINT('Ctrl Pts',(-38.7556809688784,-27.8067102122203,7.7804512420585));
#7487=CARTESIAN_POINT('Ctrl Pts',(-38.0308025912301,-28.217955439177,7.7275230023166));
#7488=CARTESIAN_POINT('Ctrl Pts',(-37.5299677902808,-29.0241095767712,7.67459476257471));
#7489=CARTESIAN_POINT('Ctrl Pts',(-37.4824296222801,-29.8561621493983,7.62166652283282));
#7490=CARTESIAN_POINT('Ctrl Pts',(-37.4348914542795,-30.6882147220254,7.56873828309093));
#7491=CARTESIAN_POINT('Ctrl Pts',(-37.8406499192275,-31.5461657296854,7.51581004334903));
#7492=CARTESIAN_POINT('Ctrl Pts',(-38.513972399747,-32.0372952238151,7.46288180360714));
#7493=CARTESIAN_POINT('Ctrl Pts',(-39.1872948802665,-32.5284247179447,7.40995356386524));
#7494=CARTESIAN_POINT('Ctrl Pts',(-40.1281813763575,-32.652732698544,7.35702532412334));
#7495=CARTESIAN_POINT('Ctrl Pts',(-40.9059488815193,-32.3533181947664,7.30409708438145));
#7496=CARTESIAN_POINT('Ctrl Pts',(-41.683716386681,-32.0539036909888,7.25116884463955));
#7497=CARTESIAN_POINT('Ctrl Pts',(-42.2983649009134,-31.3307667028344,7.19824060489766));
#7498=CARTESIAN_POINT('Ctrl Pts',(-42.4685441356896,-30.5149172235574,7.14531236515577));
#7499=CARTESIAN_POINT('Ctrl Pts',(-42.5036218614697,-30.3467524979989,7.13440267760118));
#7500=CARTESIAN_POINT('Ctrl Pts',(-42.5198156967515,-30.174648754355,7.12349299004658));
#7501=CARTESIAN_POINT('Ctrl Pts',(-42.5182251666708,-30.0022480740648,7.11258330249199));
#7502=CARTESIAN_POINT('Ctrl Pts',(-42.5135602932616,-30.0006322084125,7.38741669750801));
#7503=CARTESIAN_POINT('Ctrl Pts',(-42.5144167957854,-30.3818237747137,7.41142596246836));
#7504=CARTESIAN_POINT('Ctrl Pts',(-42.4331272831723,-30.76266867493,7.43543522742871));
#7505=CARTESIAN_POINT('Ctrl Pts',(-42.2678160640931,-31.1026604172056,7.45944449238905));
#7506=CARTESIAN_POINT('Ctrl Pts',(-41.9033887544732,-31.8521695952311,7.51237273213095));
#7507=CARTESIAN_POINT('Ctrl Pts',(-41.1306339066773,-32.4031411558927,7.56530097187284));
#7508=CARTESIAN_POINT('Ctrl Pts',(-40.3032736541046,-32.5033726170428,7.61822921161474));
#7509=CARTESIAN_POINT('Ctrl Pts',(-39.4759134015319,-32.6036040781929,7.67115745135663));
#7510=CARTESIAN_POINT('Ctrl Pts',(-38.5939477441824,-32.2530954398316,7.72408569109853));
#7511=CARTESIAN_POINT('Ctrl Pts',(-38.0610892080637,-31.6122887387886,7.77701393084043));
#7512=CARTESIAN_POINT('Ctrl Pts',(-37.5282306719451,-30.9714820377456,7.82994217058232));
#7513=CARTESIAN_POINT('Ctrl Pts',(-37.3444792570573,-30.0403772740209,7.88287041032421));
#7514=CARTESIAN_POINT('Ctrl Pts',(-37.5939455938752,-29.2451807561725,7.93579865006611));
#7515=CARTESIAN_POINT('Ctrl Pts',(-37.8434119306932,-28.4499842383242,7.988726889808));
#7516=CARTESIAN_POINT('Ctrl Pts',(-38.5260960192167,-27.7906959663523,8.04165512954989));
#7517=CARTESIAN_POINT('Ctrl Pts',(-39.3295049803966,-27.5690981165436,8.09458336929179));
#7518=CARTESIAN_POINT('Ctrl Pts',(-40.1329139415765,-27.3475002667349,8.14751160903368));
#7519=CARTESIAN_POINT('Ctrl Pts',(-41.0570477754128,-27.5635928390895,8.20043984877558));
#7520=CARTESIAN_POINT('Ctrl Pts',(-41.67889160523,-28.1184644084391,8.25336808851747));
#7521=CARTESIAN_POINT('Ctrl Pts',(-42.2038621490131,-28.586895894809,8.29805095818099));
#7522=CARTESIAN_POINT('Ctrl Pts',(-42.513390381827,-29.2967754246142,8.3427338278445));
#7523=CARTESIAN_POINT('Ctrl Pts',(-42.51946795121,-30.0019779683886,8.38741669750802));
#7524=CARTESIAN_POINT('Origin',(-40.,-30.,5.));
#7525=CARTESIAN_POINT('',(-42.5197817068771,-29.9981833838556,9.38741669750801));
#7526=CARTESIAN_POINT('',(-42.5142225916618,-29.9985870806183,9.11258330249199));
#7527=CARTESIAN_POINT('',(-42.5175,-30.,5.));
#7528=CARTESIAN_POINT('',(-38.0865340033349,-28.364012796625,10.));
#7529=CARTESIAN_POINT('Ctrl Pts',(-42.5197817068771,-29.9981833838556,9.38741669750801));
#7530=CARTESIAN_POINT('Ctrl Pts',(-42.5138583444366,-30.7144624076937,9.43282641244632));
#7531=CARTESIAN_POINT('Ctrl Pts',(-42.1929708169802,-31.4352472342186,9.47823612738463));
#7532=CARTESIAN_POINT('Ctrl Pts',(-41.6529746034879,-31.9041374282717,9.52364584232294));
#7533=CARTESIAN_POINT('Ctrl Pts',(-41.0235707614628,-32.450662167244,9.57657408206484));
#7534=CARTESIAN_POINT('Ctrl Pts',(-40.096495632782,-32.654974095277,9.62950232180673));
#7535=CARTESIAN_POINT('Ctrl Pts',(-39.2962218229396,-32.4219133635354,9.68243056154862));
#7536=CARTESIAN_POINT('Ctrl Pts',(-38.4959480130971,-32.1888526317938,9.73535880129052));
#7537=CARTESIAN_POINT('Ctrl Pts',(-37.8224755220932,-31.5184192402776,9.78828704103242));
#7538=CARTESIAN_POINT('Ctrl Pts',(-37.5841068868004,-30.7212938581909,9.84121528077432));
#7539=CARTESIAN_POINT('Ctrl Pts',(-37.3457382515077,-29.9241684761042,9.89414352051621));
#7540=CARTESIAN_POINT('Ctrl Pts',(-37.5424734719262,-29.0003511034471,9.9470717602581));
#7541=CARTESIAN_POINT('Ctrl Pts',(-38.0865340033349,-28.364012796625,10.));
#7542=CARTESIAN_POINT('',(-41.9171063737423,-28.3612428889485,9.99999999999999));
#7543=CARTESIAN_POINT('Origin',(-40.,-30.,10.));
#7544=CARTESIAN_POINT('Ctrl Pts',(-41.9171093217586,-28.3612406458477,9.99999999999999));
#7545=CARTESIAN_POINT('Ctrl Pts',(-41.3863011191192,-27.7421368159147,9.94821753066412));
#7546=CARTESIAN_POINT('Ctrl Pts',(-40.5267001215146,-27.402643603469,9.89643506132826));
#7547=CARTESIAN_POINT('Ctrl Pts',(-39.7163628817935,-27.4944831131097,9.84465259199239));
#7548=CARTESIAN_POINT('Ctrl Pts',(-38.8880956275312,-27.5883547195893,9.79172435225049));
#7549=CARTESIAN_POINT('Ctrl Pts',(-38.1112963297669,-28.1328580831711,9.73879611250859));
#7550=CARTESIAN_POINT('Ctrl Pts',(-37.741032373656,-28.8793789981345,9.6858678727667));
#7551=CARTESIAN_POINT('Ctrl Pts',(-37.3707684175451,-29.6258999130979,9.6329396330248));
#7552=CARTESIAN_POINT('Ctrl Pts',(-37.4070398030878,-30.574438379443,9.58001139328291));
#7553=CARTESIAN_POINT('Ctrl Pts',(-37.8334966681989,-31.2904958074349,9.52708315354102));
#7554=CARTESIAN_POINT('Ctrl Pts',(-38.2599535333099,-32.0065532354269,9.47415491379913));
#7555=CARTESIAN_POINT('Ctrl Pts',(-39.0765958779895,-32.4901296250657,9.42122667405723));
#7556=CARTESIAN_POINT('Ctrl Pts',(-39.9094857309799,-32.5200284649321,9.36829843431533));
#7557=CARTESIAN_POINT('Ctrl Pts',(-40.7423755839703,-32.5499273047984,9.31537019457344));
#7558=CARTESIAN_POINT('Ctrl Pts',(-41.5915129452714,-32.1261485948923,9.26244195483154));
#7559=CARTESIAN_POINT('Ctrl Pts',(-42.0682756289179,-31.4425951450394,9.20951371508965));
#7560=CARTESIAN_POINT('Ctrl Pts',(-42.3593162521113,-31.0253187329899,9.1772035775571));
#7561=CARTESIAN_POINT('Ctrl Pts',(-42.5115909448116,-30.5112369105017,9.14489344002454));
#7562=CARTESIAN_POINT('Ctrl Pts',(-42.5142225916618,-29.9985870806183,9.11258330249199));
#7563=CARTESIAN_POINT('Origin',(40.,-30.,5.));
#7564=CARTESIAN_POINT('',(37.4865493719845,-29.9993943699827,0.387416697508021));
#7565=CARTESIAN_POINT('',(37.4843806918116,-30.0035003569228,0.112583302491982));
#7566=CARTESIAN_POINT('',(37.4825,-30.,5.));
#7567=CARTESIAN_POINT('',(38.0865340033349,-28.364012796625,0.));
#7568=CARTESIAN_POINT('Ctrl Pts',(37.4843806918116,-30.0035003569228,0.112583302491982));
#7569=CARTESIAN_POINT('Ctrl Pts',(37.4896304006503,-29.4109018718323,0.0750555349946546));
#7570=CARTESIAN_POINT('Ctrl Pts',(37.700778171916,-28.8151964396956,0.0375277674973273));
#7571=CARTESIAN_POINT('Ctrl Pts',(38.0865340033349,-28.364012796625,-6.93889390390723E-17));
#7572=CARTESIAN_POINT('',(41.9171064557029,-28.361242966669,2.14205110652297E-15));
#7573=CARTESIAN_POINT('Origin',(40.,-30.,0.));
#7574=CARTESIAN_POINT('Ctrl Pts',(41.9171094063105,-28.36124072171,6.72491220257403E-16));
#7575=CARTESIAN_POINT('Ctrl Pts',(41.3863012299091,-27.7421370139191,0.0517824693358735));
#7576=CARTESIAN_POINT('Ctrl Pts',(40.526700166155,-27.4026434779206,0.103564938671746));
#7577=CARTESIAN_POINT('Ctrl Pts',(39.7163628779809,-27.4944829225585,0.155347408007619));
#7578=CARTESIAN_POINT('Ctrl Pts',(38.8880955741935,-27.5883544625971,0.208275647749513));
#7579=CARTESIAN_POINT('Ctrl Pts',(38.1112962453924,-28.132858029856,0.261203887491408));
#7580=CARTESIAN_POINT('Ctrl Pts',(37.7410322801268,-28.8793790122715,0.314132127233303));
#7581=CARTESIAN_POINT('Ctrl Pts',(37.5701428159829,-29.223923938661,0.338560317324876));
#7582=CARTESIAN_POINT('Ctrl Pts',(37.4858509825759,-29.6115013564135,0.362988507416448));
#7583=CARTESIAN_POINT('Ctrl Pts',(37.4865493719845,-29.9993943699827,0.387416697508021));
#7584=CARTESIAN_POINT('Origin',(40.,-30.,5.));
#7585=CARTESIAN_POINT('',(37.4826514345854,-30.0023034644279,1.38741669750802));
#7586=CARTESIAN_POINT('',(37.4783313032867,-29.9998786620396,1.11258330249198));
#7587=CARTESIAN_POINT('',(37.4825,-30.,5.));
#7588=CARTESIAN_POINT('Ctrl Pts',(37.4783313032867,-29.9998786620396,1.11258330249198));
#7589=CARTESIAN_POINT('Ctrl Pts',(37.4783277518435,-29.994156258084,1.11221987985458));
#7590=CARTESIAN_POINT('Ctrl Pts',(37.4783455394907,-29.9884338787842,1.11185645721719));
#7591=CARTESIAN_POINT('Ctrl Pts',(37.478384732659,-29.9827116481148,1.11149303457979));
#7592=CARTESIAN_POINT('Ctrl Pts',(37.4840927574081,-29.1493359429073,1.05856479483789));
#7593=CARTESIAN_POINT('Ctrl Pts',(37.9438226319757,-28.3191127610073,1.005636555096));
#7594=CARTESIAN_POINT('Ctrl Pts',(38.6471445572473,-27.8719690967068,0.952708315354104));
#7595=CARTESIAN_POINT('Ctrl Pts',(39.3504664825189,-27.4248254324063,0.89978007561221));
#7596=CARTESIAN_POINT('Ctrl Pts',(40.2973804584944,-27.3607612857053,0.846851835870315));
#7597=CARTESIAN_POINT('Ctrl Pts',(41.0544289594598,-27.7093027682094,0.793923596128421));
#7598=CARTESIAN_POINT('Ctrl Pts',(41.8114774604251,-28.0578442507135,0.740995356386527));
#7599=CARTESIAN_POINT('Ctrl Pts',(42.3786604863801,-28.8189913624227,0.688067116644633));
#7600=CARTESIAN_POINT('Ctrl Pts',(42.4963855115501,-29.6439332601599,0.635138876902738));
#7601=CARTESIAN_POINT('Ctrl Pts',(42.61411053672,-30.4688751578969,0.582210637160844));
#7602=CARTESIAN_POINT('Ctrl Pts',(42.2823775611047,-31.3576118416619,0.529282397418949));
#7603=CARTESIAN_POINT('Ctrl Pts',(41.6529740852769,-31.9041367057679,0.476354157677056));
#7604=CARTESIAN_POINT('Ctrl Pts',(41.023570609449,-32.4506615698739,0.42342591793516));
#7605=CARTESIAN_POINT('Ctrl Pts',(40.0964966334085,-32.6549746143208,0.370497678193266));
#7606=CARTESIAN_POINT('Ctrl Pts',(39.2962223204593,-32.4219134063263,0.317569438451371));
#7607=CARTESIAN_POINT('Ctrl Pts',(38.4959480075102,-32.1888521983318,0.264641198709478));
#7608=CARTESIAN_POINT('Ctrl Pts',(37.8224733576524,-31.5184167378959,0.211712958967584));
#7609=CARTESIAN_POINT('Ctrl Pts',(37.5841047237564,-30.7212914641747,0.158784719225691));
#7610=CARTESIAN_POINT('Ctrl Pts',(37.5147468620895,-30.4893527918657,0.143384246981121));
#7611=CARTESIAN_POINT('Ctrl Pts',(37.4822263404964,-30.2466881917031,0.127983774736552));
#7612=CARTESIAN_POINT('Ctrl Pts',(37.4843806918116,-30.0035003569228,0.112583302491982));
#7613=CARTESIAN_POINT('Ctrl Pts',(37.4865493719845,-29.9993943699827,0.387416697508021));
#7614=CARTESIAN_POINT('Ctrl Pts',(37.4873641737667,-30.4519440719579,0.415916747158343));
#7615=CARTESIAN_POINT('Ctrl Pts',(37.603864126948,-30.9049233498139,0.444416796808666));
#7616=CARTESIAN_POINT('Ctrl Pts',(37.8334965944027,-31.2904958242251,0.472916846458989));
#7617=CARTESIAN_POINT('Ctrl Pts',(38.2599534756744,-32.0065532561908,0.525845086200882));
#7618=CARTESIAN_POINT('Ctrl Pts',(39.0765958399479,-32.4901297225502,0.578773325942776));
#7619=CARTESIAN_POINT('Ctrl Pts',(39.9094857226646,-32.5200285765499,0.63170156568467));
#7620=CARTESIAN_POINT('Ctrl Pts',(40.7423756053813,-32.5499274305496,0.684629805426564));
#7621=CARTESIAN_POINT('Ctrl Pts',(41.5915130065413,-32.1261486721896,0.737558045168459));
#7622=CARTESIAN_POINT('Ctrl Pts',(42.0682757093793,-31.442595189452,0.790486284910354));
#7623=CARTESIAN_POINT('Ctrl Pts',(42.5450384122174,-30.7590417067144,0.843414524652249));
#7624=CARTESIAN_POINT('Ctrl Pts',(42.6494264167334,-29.8157134995992,0.896342764394142));
#7625=CARTESIAN_POINT('Ctrl Pts',(42.3336252269733,-29.0444504835271,0.949271004136037));
#7626=CARTESIAN_POINT('Ctrl Pts',(42.0178240372131,-28.273187467455,1.00219924387793));
#7627=CARTESIAN_POINT('Ctrl Pts',(41.2818336531767,-27.6739896424261,1.05512748361983));
#7628=CARTESIAN_POINT('Ctrl Pts',(40.462563489583,-27.5211152279163,1.10805572336172));
#7629=CARTESIAN_POINT('Ctrl Pts',(39.6432933259892,-27.3682408134066,1.16098396310362));
#7630=CARTESIAN_POINT('Ctrl Pts',(38.7407433828381,-27.6616898094161,1.21391220284551));
#7631=CARTESIAN_POINT('Ctrl Pts',(38.1680404837585,-28.2671481925974,1.26684044258741));
#7632=CARTESIAN_POINT('Ctrl Pts',(37.7331474342891,-28.7269147539535,1.30703252756094));
#7633=CARTESIAN_POINT('Ctrl Pts',(37.4884579998333,-29.3665989905621,1.34722461253448));
#7634=CARTESIAN_POINT('Ctrl Pts',(37.4826514345854,-30.0023034644279,1.38741669750802));
#7635=CARTESIAN_POINT('Origin',(40.,-30.,5.));
#7636=CARTESIAN_POINT('',(37.4786866123615,-29.9991346485264,2.38741669750802));
#7637=CARTESIAN_POINT('',(37.4841920048104,-29.9978709034909,2.11258330249198));
#7638=CARTESIAN_POINT('',(37.4825,-30.,5.));
#7639=CARTESIAN_POINT('Ctrl Pts',(37.4841920048104,-29.9978709034909,2.11258330249198));
#7640=CARTESIAN_POINT('Ctrl Pts',(37.4821417199046,-29.7423941828823,2.09645598497262));
#7641=CARTESIAN_POINT('Ctrl Pts',(37.5179332422556,-29.4874784679461,2.08032866745325));
#7642=CARTESIAN_POINT('Ctrl Pts',(37.5939460125011,-29.2451808863826,2.06420134993389));
#7643=CARTESIAN_POINT('Ctrl Pts',(37.8434123060845,-28.4499845079103,2.011273110192));
#7644=CARTESIAN_POINT('Ctrl Pts',(38.5260962765078,-27.7906963548654,1.9583448704501));
#7645=CARTESIAN_POINT('Ctrl Pts',(39.3295050974595,-27.5690985418568,1.90541663070821));
#7646=CARTESIAN_POINT('Ctrl Pts',(40.1329139184113,-27.3475007288482,1.85248839096631));
#7647=CARTESIAN_POINT('Ctrl Pts',(41.0570475898915,-27.563593255876,1.79956015122442));
#7648=CARTESIAN_POINT('Ctrl Pts',(41.6788913122662,-28.1184647318748,1.74663191148252));
#7649=CARTESIAN_POINT('Ctrl Pts',(42.300735034641,-28.6733362078736,1.69370367174063));
#7650=CARTESIAN_POINT('Ctrl Pts',(42.6202888079102,-29.5669866328433,1.64077543199873));
#7651=CARTESIAN_POINT('Ctrl Pts',(42.4912800198408,-30.3903485605237,1.58784719225684));
#7652=CARTESIAN_POINT('Ctrl Pts',(42.3622712317715,-31.2137104882041,1.53491895251494));
#7653=CARTESIAN_POINT('Ctrl Pts',(41.7846998823636,-31.9667839185952,1.48199071277305));
#7654=CARTESIAN_POINT('Ctrl Pts',(41.0229435118419,-32.3048683773518,1.42906247303116));
#7655=CARTESIAN_POINT('Ctrl Pts',(40.2611871413201,-32.6429528361084,1.37613423328926));
#7656=CARTESIAN_POINT('Ctrl Pts',(39.3152457496845,-32.5660483232304,1.32320599354737));
#7657=CARTESIAN_POINT('Ctrl Pts',(38.6181181413319,-32.1093319525339,1.27027775380547));
#7658=CARTESIAN_POINT('Ctrl Pts',(37.9257772395706,-31.6557515460937,1.21771293670098));
#7659=CARTESIAN_POINT('Ctrl Pts',(37.4788449778475,-30.8275572003943,1.16514811959648));
#7660=CARTESIAN_POINT('Ctrl Pts',(37.4783313032867,-29.9998786620396,1.11258330249198));
#7661=CARTESIAN_POINT('Ctrl Pts',(37.4826514345854,-30.0023034644279,1.38741669750802));
#7662=CARTESIAN_POINT('Ctrl Pts',(37.4808114376377,-30.2037468722884,1.40015285227638));
#7663=CARTESIAN_POINT('Ctrl Pts',(37.5029586978307,-30.4047906550415,1.41288900704473));
#7664=CARTESIAN_POINT('Ctrl Pts',(37.5506421647824,-30.5995832878214,1.42562516181309));
#7665=CARTESIAN_POINT('Ctrl Pts',(37.748802599894,-31.4090922295111,1.47855340155498));
#7666=CARTESIAN_POINT('Ctrl Pts',(38.3879793251253,-32.1106423425376,1.53148164129688));
#7667=CARTESIAN_POINT('Ctrl Pts',(39.1755924790674,-32.3831073213503,1.58440988103877));
#7668=CARTESIAN_POINT('Ctrl Pts',(39.9632056330096,-32.6555723001631,1.63733812078066));
#7669=CARTESIAN_POINT('Ctrl Pts',(40.8992552156624,-32.4989521447621,1.69026636052256));
#7670=CARTESIAN_POINT('Ctrl Pts',(41.5552732606538,-31.9849372039589,1.74319460026445));
#7671=CARTESIAN_POINT('Ctrl Pts',(42.2112913056452,-31.4709222631558,1.79612284000635));
#7672=CARTESIAN_POINT('Ctrl Pts',(42.587277812975,-30.5995125369504,1.84905107974824));
#7673=CARTESIAN_POINT('Ctrl Pts',(42.5111275644027,-29.7695892476869,1.90197931949014));
#7674=CARTESIAN_POINT('Ctrl Pts',(42.4349773158305,-28.9396659584235,1.95490755923203));
#7675=CARTESIAN_POINT('Ctrl Pts',(41.9066903113561,-28.151229106102,2.00783579897393));
#7676=CARTESIAN_POINT('Ctrl Pts',(41.1680858141738,-27.7651788384674,2.06076403871582));
#7677=CARTESIAN_POINT('Ctrl Pts',(40.4294813169916,-27.3791285708329,2.11369227845772));
#7678=CARTESIAN_POINT('Ctrl Pts',(39.4805593271014,-27.3954648878851,2.16662051819961));
#7679=CARTESIAN_POINT('Ctrl Pts',(38.7556809223357,-27.8067101302471,2.21954875794151));
#7680=CARTESIAN_POINT('Ctrl Pts',(38.0308025175699,-28.217955372609,2.2724769976834));
#7681=CARTESIAN_POINT('Ctrl Pts',(37.5299676979286,-29.0241095402806,2.3254052374253));
#7682=CARTESIAN_POINT('Ctrl Pts',(37.4824295281584,-29.8561621440027,2.37833347716719));
#7683=CARTESIAN_POINT('Ctrl Pts',(37.4797101249769,-29.9037594012931,2.3813612172808));
#7684=CARTESIAN_POINT('Ctrl Pts',(37.4784740757625,-29.9514414078264,2.38438895739441));
#7685=CARTESIAN_POINT('Ctrl Pts',(37.4786866123615,-29.9991346485264,2.38741669750802));
#7686=CARTESIAN_POINT('Origin',(40.,-30.,5.));
#7687=CARTESIAN_POINT('',(37.4852131002495,-29.9982362785157,3.38741669750802));
#7688=CARTESIAN_POINT('',(37.4858831881014,-30.0013301674969,3.11258330249199));
#7689=CARTESIAN_POINT('',(37.4825,-30.,5.));
#7690=CARTESIAN_POINT('Ctrl Pts',(37.4858831881014,-30.0013301674969,3.11258330249199));
#7691=CARTESIAN_POINT('Ctrl Pts',(37.4883078730657,-29.4952785276618,3.08069209009065));
#7692=CARTESIAN_POINT('Ctrl Pts',(37.636378023608,-28.987921426998,3.04880087768932));
#7693=CARTESIAN_POINT('Ctrl Pts',(37.9203890614956,-28.5737932182074,3.01690966528799));
#7694=CARTESIAN_POINT('Ctrl Pts',(38.3917478832765,-27.8864854782912,2.96398142554609));
#7695=CARTESIAN_POINT('Ctrl Pts',(39.2375473130611,-27.4559708463078,2.9110531858042));
#7696=CARTESIAN_POINT('Ctrl Pts',(40.0706296497584,-27.4793138140309,2.85812494606231));
#7697=CARTESIAN_POINT('Ctrl Pts',(40.9037119864556,-27.502656781754,2.80519670632041));
#7698=CARTESIAN_POINT('Ctrl Pts',(41.7240772300655,-27.9798573491834,2.75226846657852));
#7699=CARTESIAN_POINT('Ctrl Pts',(42.1562099623478,-28.6924809482542,2.69934022683662));
#7700=CARTESIAN_POINT('Ctrl Pts',(42.5883426946301,-29.4051045473249,2.64641198709473));
#7701=CARTESIAN_POINT('Ctrl Pts',(42.6322429155848,-30.353151178037,2.59348374735284));
#7702=CARTESIAN_POINT('Ctrl Pts',(42.2678156693759,-31.1026602254528,2.54055550761094));
#7703=CARTESIAN_POINT('Ctrl Pts',(41.903388423167,-31.8521692728685,2.48762726786905));
#7704=CARTESIAN_POINT('Ctrl Pts',(41.1306337097946,-32.4031407369879,2.43469902812715));
#7705=CARTESIAN_POINT('Ctrl Pts',(40.3032736012765,-32.503372180972,2.38177078838526));
#7706=CARTESIAN_POINT('Ctrl Pts',(39.4759134927584,-32.6036036249562,2.32884254864336));
#7707=CARTESIAN_POINT('Ctrl Pts',(38.5939479890946,-32.2530950488052,2.27591430890147));
#7708=CARTESIAN_POINT('Ctrl Pts',(38.0610895456344,-31.6122884587799,2.22298606915957));
#7709=CARTESIAN_POINT('Ctrl Pts',(37.6905939041957,-31.1667366400493,2.18618514693704));
#7710=CARTESIAN_POINT('Ctrl Pts',(37.4888705494763,-30.5808431748248,2.14938422471451));
#7711=CARTESIAN_POINT('Ctrl Pts',(37.4841920048104,-29.9978709034909,2.11258330249198));
#7712=CARTESIAN_POINT('Ctrl Pts',(37.4786866123615,-29.9991346485264,2.38741669750802));
#7713=CARTESIAN_POINT('Ctrl Pts',(37.4821894501486,-30.7851719075128,2.43731719713631));
#7714=CARTESIAN_POINT('Ctrl Pts',(37.8791670000235,-31.5742606671538,2.48721769676459));
#7715=CARTESIAN_POINT('Ctrl Pts',(38.5139723441797,-32.0372952999983,2.53711819639287));
#7716=CARTESIAN_POINT('Ctrl Pts',(39.1872948498703,-32.5284248124992,2.59004643613477));
#7717=CARTESIAN_POINT('Ctrl Pts',(40.1281813811507,-32.6527327977285,2.64297467587666));
#7718=CARTESIAN_POINT('Ctrl Pts',(40.9059489153952,-32.3533182827517,2.69590291561856));
#7719=CARTESIAN_POINT('Ctrl Pts',(41.6837164496398,-32.0539037677748,2.74883115536045));
#7720=CARTESIAN_POINT('Ctrl Pts',(42.2983649868485,-31.3307667525918,2.80175939510234));
#7721=CARTESIAN_POINT('Ctrl Pts',(42.4685442279864,-30.5149172428125,2.85468763484424));
#7722=CARTESIAN_POINT('Ctrl Pts',(42.6387234691244,-29.6990677330333,2.90761587458613));
#7723=CARTESIAN_POINT('Ctrl Pts',(42.3644334141915,-28.7905057286578,2.96054411432803));
#7724=CARTESIAN_POINT('Ctrl Pts',(41.7712280742516,-28.2051179779666,3.01347235406992));
#7725=CARTESIAN_POINT('Ctrl Pts',(41.1780227343116,-27.6197302272753,3.06640059381182));
#7726=CARTESIAN_POINT('Ctrl Pts',(40.2659021093645,-27.3575167302683,3.11932883355372));
#7727=CARTESIAN_POINT('Ctrl Pts',(39.4523818797609,-27.5385035518619,3.17225707329561));
#7728=CARTESIAN_POINT('Ctrl Pts',(38.6388616501573,-27.7194903734554,3.2251853130375));
#7729=CARTESIAN_POINT('Ctrl Pts',(37.9239418158972,-28.3436775136496,3.2781135527794));
#7730=CARTESIAN_POINT('Ctrl Pts',(37.6348710271545,-29.1253484633316,3.33104179252129));
#7731=CARTESIAN_POINT('Ctrl Pts',(37.532239373874,-29.4028728103475,3.34983342751687));
#7732=CARTESIAN_POINT('Ctrl Pts',(37.4832873999723,-29.7002485119447,3.36862506251244));
#7733=CARTESIAN_POINT('Ctrl Pts',(37.4852131002495,-29.9982362785157,3.38741669750802));
#7734=CARTESIAN_POINT('Origin',(40.,-30.,5.));
#7735=CARTESIAN_POINT('',(37.4850673154095,-30.0018328376965,4.38741669750802));
#7736=CARTESIAN_POINT('',(37.4793388029256,-30.0014234821656,4.11258330249199));
#7737=CARTESIAN_POINT('',(37.4825,-30.,5.));
#7738=CARTESIAN_POINT('Ctrl Pts',(37.4793388029256,-30.0014234821656,4.11258330249199));
#7739=CARTESIAN_POINT('Ctrl Pts',(37.4844209002651,-29.2502423854113,4.06492819520869));
#7740=CARTESIAN_POINT('Ctrl Pts',(37.8421140990601,-28.4948609126137,4.01727308792539));
#7741=CARTESIAN_POINT('Ctrl Pts',(38.4291014552389,-28.0274064804584,3.96961798064209));
#7742=CARTESIAN_POINT('Ctrl Pts',(39.0810401305334,-27.5082272851111,3.9166897409002));
#7743=CARTESIAN_POINT('Ctrl Pts',(40.0158241190993,-27.3442198697122,3.86376150115831));
#7744=CARTESIAN_POINT('Ctrl Pts',(40.8055637711363,-27.610457273629,3.81083326141641));
#7745=CARTESIAN_POINT('Ctrl Pts',(41.5953034231733,-27.8766946775457,3.75790502167452));
#7746=CARTESIAN_POINT('Ctrl Pts',(42.2399987386814,-28.5731769007781,3.70497678193262));
#7747=CARTESIAN_POINT('Ctrl Pts',(42.4445457618467,-29.3810949590939,3.65204854219072));
#7748=CARTESIAN_POINT('Ctrl Pts',(42.6490927850121,-30.1890130174097,3.59912030244883));
#7749=CARTESIAN_POINT('Ctrl Pts',(42.4134915158347,-31.1083669108089,3.54619206270694));
#7750=CARTESIAN_POINT('Ctrl Pts',(41.8455864894317,-31.7183299864945,3.49326382296504));
#7751=CARTESIAN_POINT('Ctrl Pts',(41.2776814630286,-32.3282930621801,3.44033558322315));
#7752=CARTESIAN_POINT('Ctrl Pts',(40.3774726793999,-32.628865320152,3.38740734348125));
#7753=CARTESIAN_POINT('Ctrl Pts',(39.5570232736503,-32.4824622950877,3.33447910373936));
#7754=CARTESIAN_POINT('Ctrl Pts',(38.7365738679008,-32.3360592700233,3.28155086399746));
#7755=CARTESIAN_POINT('Ctrl Pts',(37.9958838400304,-31.7426809619227,3.22862262425557));
#7756=CARTESIAN_POINT('Ctrl Pts',(37.6739979329839,-30.9739413839478,3.17569438451368));
#7757=CARTESIAN_POINT('Ctrl Pts',(37.5460601315361,-30.6683956941894,3.15465735717311));
#7758=CARTESIAN_POINT('Ctrl Pts',(37.484283745495,-30.3351469584353,3.13362032983255));
#7759=CARTESIAN_POINT('Ctrl Pts',(37.4858831881014,-30.0013301674969,3.11258330249199));
#7760=CARTESIAN_POINT('Ctrl Pts',(37.4852131002495,-29.9982362785157,3.38741669750802));
#7761=CARTESIAN_POINT('Ctrl Pts',(37.4887112987426,-30.5395564249036,3.42155330225434));
#7762=CARTESIAN_POINT('Ctrl Pts',(37.6601048829887,-31.0828963744086,3.45568990700066));
#7763=CARTESIAN_POINT('Ctrl Pts',(37.9825966796778,-31.5129224074782,3.48982651174697));
#7764=CARTESIAN_POINT('Ctrl Pts',(38.4826148641692,-32.179670642773,3.54275475148887));
#7765=CARTESIAN_POINT('Ctrl Pts',(39.3458729763774,-32.5740123541928,3.59568299123076));
#7766=CARTESIAN_POINT('Ctrl Pts',(40.1772217458474,-32.5154408801314,3.64861123097266));
#7767=CARTESIAN_POINT('Ctrl Pts',(41.0085705153174,-32.4568694060699,3.70153947071455));
#7768=CARTESIAN_POINT('Ctrl Pts',(41.8080099420493,-31.9453847465272,3.75446771045645));
#7769=CARTESIAN_POINT('Ctrl Pts',(42.2096032313768,-31.2151147799068,3.80739595019834));
#7770=CARTESIAN_POINT('Ctrl Pts',(42.6111965207043,-30.4848448132865,3.86032418994024));
#7771=CARTESIAN_POINT('Ctrl Pts',(42.6149436726274,-29.5357895395886,3.91325242968213));
#7772=CARTESIAN_POINT('Ctrl Pts',(42.2191294593654,-28.8023711714614,3.96618066942403));
#7773=CARTESIAN_POINT('Ctrl Pts',(41.8233152461034,-28.0689528033342,4.01910890916592));
#7774=CARTESIAN_POINT('Ctrl Pts',(41.0279396676562,-27.5511713407776,4.07203714890781));
#7775=CARTESIAN_POINT('Ctrl Pts',(40.1970793255485,-27.4860369716512,4.12496538864971));
#7776=CARTESIAN_POINT('Ctrl Pts',(39.3662189834407,-27.4209026025248,4.1778936283916));
#7777=CARTESIAN_POINT('Ctrl Pts',(38.4998738776723,-27.8084153268287,4.2308218681335));
#7778=CARTESIAN_POINT('Ctrl Pts',(37.9946063247663,-28.4711943956907,4.2837501078754));
#7779=CARTESIAN_POINT('Ctrl Pts',(37.6647297200325,-28.9039063473437,4.31830563775294));
#7780=CARTESIAN_POINT('Ctrl Pts',(37.4887609409795,-29.4539494491559,4.35286116763048));
#7781=CARTESIAN_POINT('Ctrl Pts',(37.4850673154095,-30.0018328376965,4.38741669750802));
#7782=CARTESIAN_POINT('Origin',(40.,-30.,5.));
#7783=CARTESIAN_POINT('',(37.4785971457328,-30.0007512051729,5.38741669750803));
#7784=CARTESIAN_POINT('',(37.4815747780937,-29.9977798171256,5.11258330249199));
#7785=CARTESIAN_POINT('',(37.4825,-30.,5.));
#7786=CARTESIAN_POINT('Ctrl Pts',(37.4815747780937,-29.9977798171256,5.11258330249199));
#7787=CARTESIAN_POINT('Ctrl Pts',(37.4800513919894,-29.8320332010168,5.10209254006862));
#7788=CARTESIAN_POINT('Ctrl Pts',(37.4950144905386,-29.6665602978234,5.09160177764525));
#7789=CARTESIAN_POINT('Ctrl Pts',(37.5274672786068,-29.5045917111079,5.08111101522188));
#7790=CARTESIAN_POINT('Ctrl Pts',(37.691198843373,-28.6874240122915,5.02818277547998));
#7791=CARTESIAN_POINT('Ctrl Pts',(38.3001178421193,-27.9594561622746,4.97525453573809));
#7792=CARTESIAN_POINT('Ctrl Pts',(39.075496632593,-27.6539094316881,4.92232629599619));
#7793=CARTESIAN_POINT('Ctrl Pts',(39.8508754230667,-27.3483627011017,4.8693980562543));
#7794=CARTESIAN_POINT('Ctrl Pts',(40.7927140052677,-27.4652370899456,4.81646981651241));
#7795=CARTESIAN_POINT('Ctrl Pts',(41.4698935473972,-27.9510343120548,4.76354157677051));
#7796=CARTESIAN_POINT('Ctrl Pts',(42.1470730895267,-28.4368315341641,4.71061333702862));
#7797=CARTESIAN_POINT('Ctrl Pts',(42.5595935915846,-29.2915515895388,4.65768509728672));
#7798=CARTESIAN_POINT('Ctrl Pts',(42.5186272010046,-30.1239534324835,4.60475685754483));
#7799=CARTESIAN_POINT('Ctrl Pts',(42.4776608104246,-30.9563552754283,4.55182861780293));
#7800=CARTESIAN_POINT('Ctrl Pts',(41.9832075272066,-31.7664389059432,4.49890037806104));
#7801=CARTESIAN_POINT('Ctrl Pts',(41.2615992577626,-32.183395233096,4.44597213831914));
#7802=CARTESIAN_POINT('Ctrl Pts',(40.5399909883187,-32.6003515602488,4.39304389857725));
#7803=CARTESIAN_POINT('Ctrl Pts',(39.5912277326488,-32.6241805840396,4.34011565883535));
#7804=CARTESIAN_POINT('Ctrl Pts',(38.8495980346337,-32.243974765696,4.28718741909346));
#7805=CARTESIAN_POINT('Ctrl Pts',(38.1079683366186,-31.8637689473525,4.23425917935157));
#7806=CARTESIAN_POINT('Ctrl Pts',(37.5734721962583,-31.0795282868747,4.18133093960967));
#7807=CARTESIAN_POINT('Ctrl Pts',(37.4907708070897,-30.250232468988,4.12840269986778));
#7808=CARTESIAN_POINT('Ctrl Pts',(37.4825314365435,-30.1676114198769,4.12312956740918));
#7809=CARTESIAN_POINT('Ctrl Pts',(37.4787764587412,-30.0845431654355,4.11785643495059));
#7810=CARTESIAN_POINT('Ctrl Pts',(37.4793388029256,-30.0014234821656,4.11258330249199));
#7811=CARTESIAN_POINT('Ctrl Pts',(37.4850673154095,-30.0018328376965,4.38741669750802));
#7812=CARTESIAN_POINT('Ctrl Pts',(37.4831034644373,-30.2931350568442,4.40578940737237));
#7813=CARTESIAN_POINT('Ctrl Pts',(37.5298401746273,-30.5838267454182,4.42416211723672));
#7814=CARTESIAN_POINT('Ctrl Pts',(37.6280381061972,-30.8559480958414,4.44253482710107));
#7815=CARTESIAN_POINT('Ctrl Pts',(37.9109274405776,-31.6398773137099,4.49546306684297));
#7816=CARTESIAN_POINT('Ctrl Pts',(38.6208961093818,-32.2696903360266,4.54839130658486));
#7817=CARTESIAN_POINT('Ctrl Pts',(39.4329618185209,-32.4570954538202,4.60131954632676));
#7818=CARTESIAN_POINT('Ctrl Pts',(40.24502752766,-32.6445005716137,4.65424778606865));
#7819=CARTESIAN_POINT('Ctrl Pts',(41.1591902771339,-32.389497784884,4.70717602581055));
#7820=CARTESIAN_POINT('Ctrl Pts',(41.7569996189814,-31.8088125130406,4.76010426555244));
#7821=CARTESIAN_POINT('Ctrl Pts',(42.3548089608288,-31.2281272411973,4.81303250529434));
#7822=CARTESIAN_POINT('Ctrl Pts',(42.6362648950499,-30.3217594842401,4.86596074503623));
#7823=CARTESIAN_POINT('Ctrl Pts',(42.4725332924671,-29.5045915966848,4.91888898477813));
#7824=CARTESIAN_POINT('Ctrl Pts',(42.3088016898843,-28.6874237091295,4.97181722452002));
#7825=CARTESIAN_POINT('Ctrl Pts',(41.6998825504976,-27.959455690976,5.02474546426192));
#7826=CARTESIAN_POINT('Ctrl Pts',(40.9245035809369,-27.6539088898183,5.07767370400381));
#7827=CARTESIAN_POINT('Ctrl Pts',(40.1491246113762,-27.3483620886605,5.1306019437457));
#7828=CARTESIAN_POINT('Ctrl Pts',(39.2072858116414,-27.4652365044985,5.1835301834876));
#7829=CARTESIAN_POINT('Ctrl Pts',(38.5301061131057,-27.951033838811,5.23645842322949));
#7830=CARTESIAN_POINT('Ctrl Pts',(37.8863043721956,-28.4128863873091,5.286777847989));
#7831=CARTESIAN_POINT('Ctrl Pts',(37.4817147993667,-29.208189970679,5.33709727274851));
#7832=CARTESIAN_POINT('Ctrl Pts',(37.4785971457328,-30.0007512051729,5.38741669750803));
#7833=CARTESIAN_POINT('Origin',(40.,-30.,5.));
#7834=CARTESIAN_POINT('',(37.4828504064482,-29.9976988315479,6.38741669750802));
#7835=CARTESIAN_POINT('',(37.4865857580008,-29.9999453848463,6.11258330249199));
#7836=CARTESIAN_POINT('',(37.4825,-30.,5.));
#7837=CARTESIAN_POINT('Ctrl Pts',(37.4865857580008,-29.9999453848463,6.11258330249199));
#7838=CARTESIAN_POINT('Ctrl Pts',(37.4865051054086,-29.5830438800611,6.08632864518665));
#7839=CARTESIAN_POINT('Ctrl Pts',(37.5845304195934,-29.1661780579881,6.06007398788132));
#7840=CARTESIAN_POINT('Ctrl Pts',(37.7808710531806,-28.8023714480745,6.03381933057598));
#7841=CARTESIAN_POINT('Ctrl Pts',(38.1766851750226,-28.0689532493429,5.98089109083409));
#7842=CARTESIAN_POINT('Ctrl Pts',(38.972060569764,-27.5511719063765,5.92796285109219));
#7843=CARTESIAN_POINT('Ctrl Pts',(39.8029207199703,-27.4860375522939,5.8750346113503));
#7844=CARTESIAN_POINT('Ctrl Pts',(40.6337808701766,-27.4209031982113,5.8221063716084));
#7845=CARTESIAN_POINT('Ctrl Pts',(41.5001257758479,-27.8084158330126,5.76917813186651));
#7846=CARTESIAN_POINT('Ctrl Pts',(42.0053932120537,-28.4711947487945,5.71624989212461));
#7847=CARTESIAN_POINT('Ctrl Pts',(42.5106606482595,-29.1339736645764,5.66332165238272));
#7848=CARTESIAN_POINT('Ctrl Pts',(42.6548506149998,-30.0720188613389,5.61039341264082));
#7849=CARTESIAN_POINT('Ctrl Pts',(42.3719613459576,-30.8559478981455,5.55746517289893));
#7850=CARTESIAN_POINT('Ctrl Pts',(42.0890720769154,-31.6398769349521,5.50453693315703));
#7851=CARTESIAN_POINT('Ctrl Pts',(41.3791035720906,-32.2696898118028,5.45160869341514));
#7852=CARTESIAN_POINT('Ctrl Pts',(40.5670380505119,-32.4570948863119,5.39868045367324));
#7853=CARTESIAN_POINT('Ctrl Pts',(39.7549725289333,-32.6444999608211,5.34575221393135));
#7854=CARTESIAN_POINT('Ctrl Pts',(38.8408099906009,-32.3894972329887,5.29282397418945));
#7855=CARTESIAN_POINT('Ctrl Pts',(38.2430007868277,-31.8088120952645,5.23989573444756));
#7856=CARTESIAN_POINT('Ctrl Pts',(37.7636817191685,-31.3432229791037,5.19745825712904));
#7857=CARTESIAN_POINT('Ctrl Pts',(37.4877372151636,-30.6682619020185,5.15502077981051));
#7858=CARTESIAN_POINT('Ctrl Pts',(37.4815747780937,-29.9977798171256,5.11258330249199));
#7859=CARTESIAN_POINT('Ctrl Pts',(37.4785971457328,-30.0007512051729,5.38741669750803));
#7860=CARTESIAN_POINT('Ctrl Pts',(37.4784355107072,-30.0418416117681,5.39002551249041));
#7861=CARTESIAN_POINT('Ctrl Pts',(37.4793529973139,-30.0829246471678,5.39263432747279));
#7862=CARTESIAN_POINT('Ctrl Pts',(37.4813722172753,-30.1239534611127,5.39524314245518));
#7863=CARTESIAN_POINT('Ctrl Pts',(37.5223386173172,-30.956355496315,5.44817138219707));
#7864=CARTESIAN_POINT('Ctrl Pts',(38.0167920147376,-31.7664393139323,5.50109962193897));
#7865=CARTESIAN_POINT('Ctrl Pts',(38.7384004508494,-32.1833957373885,5.55402786168086));
#7866=CARTESIAN_POINT('Ctrl Pts',(39.4600088869611,-32.6003521608446,5.60695610142275));
#7867=CARTESIAN_POINT('Ctrl Pts',(40.4087723617641,-32.6241811901395,5.65988434116465));
#7868=CARTESIAN_POINT('Ctrl Pts',(41.1504022310713,-32.2439752839807,5.71281258090654));
#7869=CARTESIAN_POINT('Ctrl Pts',(41.8920321003785,-31.8637693778219,5.76574082064844));
#7870=CARTESIAN_POINT('Ctrl Pts',(42.42652836419,-31.0795285362096,5.81866906039033));
#7871=CARTESIAN_POINT('Ctrl Pts',(42.5092297724598,-30.2502325267831,5.87159730013223));
#7872=CARTESIAN_POINT('Ctrl Pts',(42.5919311807296,-29.4209365173566,5.92452553987412));
#7873=CARTESIAN_POINT('Ctrl Pts',(42.2228377334579,-28.5465853401159,5.97745377961602));
#7874=CARTESIAN_POINT('Ctrl Pts',(41.570898907587,-28.0274060248547,6.03038201935791));
#7875=CARTESIAN_POINT('Ctrl Pts',(40.9189600817161,-27.5082267095935,6.08331025909981));
#7876=CARTESIAN_POINT('Ctrl Pts',(39.984175877246,-27.3442192563117,6.1362384988417));
#7877=CARTESIAN_POINT('Ctrl Pts',(39.194436042805,-27.6104567217217,6.18916673858359));
#7878=CARTESIAN_POINT('Ctrl Pts',(38.404696208364,-27.8766941871318,6.24209497832549));
#7879=CARTESIAN_POINT('Ctrl Pts',(37.7600007439522,-28.5731765712337,6.29502321806739));
#7880=CARTESIAN_POINT('Ctrl Pts',(37.5554536735433,-29.3810948161497,6.34795145780928));
#7881=CARTESIAN_POINT('Ctrl Pts',(37.5046144038534,-29.5818993227048,6.36110653770886));
#7882=CARTESIAN_POINT('Ctrl Pts',(37.4809652589362,-29.7895877688607,6.37426161760844));
#7883=CARTESIAN_POINT('Ctrl Pts',(37.4828504064482,-29.9976988315479,6.38741669750802));
#7884=CARTESIAN_POINT('Origin',(40.,-30.,5.));
#7885=CARTESIAN_POINT('',(37.4864395637057,-30.0006322084003,7.38741669750802));
#7886=CARTESIAN_POINT('',(37.4817753207913,-30.0022480736136,7.11258330249199));
#7887=CARTESIAN_POINT('',(37.4825,-30.,5.));
#7888=CARTESIAN_POINT('Ctrl Pts',(37.4817753207913,-30.0022480736136,7.11258330249199));
#7889=CARTESIAN_POINT('Ctrl Pts',(37.4879012302583,-29.3382487112704,7.07056475030469));
#7890=CARTESIAN_POINT('Ctrl Pts',(37.7578399195865,-28.6698445990111,7.02854619811738));
#7891=CARTESIAN_POINT('Ctrl Pts',(38.2287723348486,-28.2051183925334,6.98652764593008));
#7892=CARTESIAN_POINT('Ctrl Pts',(38.8219775377818,-27.6197307770547,6.93359940618819));
#7893=CARTESIAN_POINT('Ctrl Pts',(39.7340979520498,-27.3575173405945,6.88067116644629));
#7894=CARTESIAN_POINT('Ctrl Pts',(40.5476179937548,-27.5385041203823,6.82774292670439));
#7895=CARTESIAN_POINT('Ctrl Pts',(41.3611380354598,-27.7194909001701,6.7748146869625));
#7896=CARTESIAN_POINT('Ctrl Pts',(42.0760577046018,-28.3436778962059,6.72188644722061));
#7897=CARTESIAN_POINT('Ctrl Pts',(42.3651284265798,-29.1253486653496,6.66895820747872));
#7898=CARTESIAN_POINT('Ctrl Pts',(42.6541991485579,-29.9070194344933,6.61602996773682));
#7899=CARTESIAN_POINT('Ctrl Pts',(42.517420923372,-30.8461739767449,6.56310172799492));
#7900=CARTESIAN_POINT('Ctrl Pts',(42.0174028543677,-31.5129220580417,6.51017348825303));
#7901=CARTESIAN_POINT('Ctrl Pts',(41.5173847853634,-32.1796701393386,6.45724524851113));
#7902=CARTESIAN_POINT('Ctrl Pts',(40.6541268725408,-32.5740117596807,6.40431700876924));
#7903=CARTESIAN_POINT('Ctrl Pts',(39.8227782950853,-32.5154402991479,6.35138876902734));
#7904=CARTESIAN_POINT('Ctrl Pts',(38.9914297176298,-32.4568688386151,6.29846052928545));
#7905=CARTESIAN_POINT('Ctrl Pts',(38.1919904755415,-31.9453842972072,6.24553228954355));
#7906=CARTESIAN_POINT('Ctrl Pts',(37.7903972789686,-31.215114499255,6.19260404980166));
#7907=CARTESIAN_POINT('Ctrl Pts',(37.5880113827631,-30.8470895705667,6.1659304673651));
#7908=CARTESIAN_POINT('Ctrl Pts',(37.4866676975036,-30.4234990624467,6.13925688492854));
#7909=CARTESIAN_POINT('Ctrl Pts',(37.4865857580008,-29.9999453848463,6.11258330249199));
#7910=CARTESIAN_POINT('Ctrl Pts',(37.4828504064482,-29.9976988315479,6.38741669750802));
#7911=CARTESIAN_POINT('Ctrl Pts',(37.4885499745158,-30.6269032624138,6.42718985735033));
#7912=CARTESIAN_POINT('Ctrl Pts',(37.7276582419413,-31.2599708265612,6.46696301719264));
#7913=CARTESIAN_POINT('Ctrl Pts',(38.1544130842988,-31.7183303833674,6.50673617703496));
#7914=CARTESIAN_POINT('Ctrl Pts',(38.7223182418689,-32.3282935999387,6.55966441677685));
#7915=CARTESIAN_POINT('Ctrl Pts',(39.6225272334149,-32.6288659273512,6.61259265651875));
#7916=CARTESIAN_POINT('Ctrl Pts',(40.4429768286621,-32.4824628684643,6.66552089626065));
#7917=CARTESIAN_POINT('Ctrl Pts',(41.2634264239092,-32.3360598095774,6.71844913600254));
#7918=CARTESIAN_POINT('Ctrl Pts',(42.0041166228575,-31.742681364391,6.77137737574443));
#7919=CARTESIAN_POINT('Ctrl Pts',(42.3260026042476,-30.9739416088782,6.82430561548633));
#7920=CARTESIAN_POINT('Ctrl Pts',(42.6478885856377,-30.2052018533655,6.87723385522822));
#7921=CARTESIAN_POINT('Ctrl Pts',(42.5509703494696,-29.2611007875262,6.93016209497012));
#7922=CARTESIAN_POINT('Ctrl Pts',(42.0796114188234,-28.5737928888347,6.98309033471202));
#7923=CARTESIAN_POINT('Ctrl Pts',(41.6082524881772,-27.8864849901432,7.03601857445391));
#7924=CARTESIAN_POINT('Ctrl Pts',(40.762452863053,-27.4559702585993,7.0889468141958));
#7925=CARTESIAN_POINT('Ctrl Pts',(39.9293703339345,-27.4793132317701,7.1418750539377));
#7926=CARTESIAN_POINT('Ctrl Pts',(39.096287804816,-27.5026562049409,7.19480329367959));
#7927=CARTESIAN_POINT('Ctrl Pts',(38.2759223717032,-27.9798568828263,7.24773153342148));
#7928=CARTESIAN_POINT('Ctrl Pts',(37.8437895396261,-28.6924806463837,7.30065977316338));
#7929=CARTESIAN_POINT('Ctrl Pts',(37.6076804505263,-29.0818445993046,7.32957874794493));
#7930=CARTESIAN_POINT('Ctrl Pts',(37.4874712144567,-29.5414898757325,7.35849772272648));
#7931=CARTESIAN_POINT('Ctrl Pts',(37.4864395637057,-30.0006322084003,7.38741669750802));
#7932=CARTESIAN_POINT('Origin',(40.,-30.,5.));
#7933=CARTESIAN_POINT('',(37.4805319060517,-30.0019779656107,8.38741669750802));
#7934=CARTESIAN_POINT('',(37.4791974871636,-29.9986726512116,8.11258330249198));
#7935=CARTESIAN_POINT('',(37.4825,-30.,5.));
#7936=CARTESIAN_POINT('Ctrl Pts',(37.4791974871636,-29.9986726512116,8.11258330249198));
#7937=CARTESIAN_POINT('Ctrl Pts',(37.478708128852,-29.9221677179019,8.10772909516461));
#7938=CARTESIAN_POINT('Ctrl Pts',(37.4818890495647,-29.8457040321827,8.10287488783723));
#7939=CARTESIAN_POINT('Ctrl Pts',(37.4888730152059,-29.7695893001576,8.09802068050986));
#7940=CARTESIAN_POINT('Ctrl Pts',(37.565023245898,-28.9396662019417,8.04509244076796));
#7941=CARTESIAN_POINT('Ctrl Pts',(38.0933101290704,-28.1512295331621,7.99216420102607));
#7942=CARTESIAN_POINT('Ctrl Pts',(38.8319144558216,-27.7651793550315,7.93923596128418));
#7943=CARTESIAN_POINT('Ctrl Pts',(39.5705187825728,-27.379129176901,7.88630772154229));
#7944=CARTESIAN_POINT('Ctrl Pts',(40.5194405529029,-27.3954654894196,7.83337948180039));
#7945=CARTESIAN_POINT('Ctrl Pts',(41.2443187901563,-27.8067106366176,7.7804512420585));
#7946=CARTESIAN_POINT('Ctrl Pts',(41.9691970274096,-28.2179557838156,7.72752300231661));
#7947=CARTESIAN_POINT('Ctrl Pts',(42.4700317315862,-29.024109765693,7.67459476257471));
#7948=CARTESIAN_POINT('Ctrl Pts',(42.5175698904255,-29.8561621773333,7.62166652283281));
#7949=CARTESIAN_POINT('Ctrl Pts',(42.5651080492647,-30.6882145889737,7.56873828309092));
#7950=CARTESIAN_POINT('Ctrl Pts',(42.1593496627666,-31.546165430377,7.51581004334902));
#7951=CARTESIAN_POINT('Ctrl Pts',(41.4860273125649,-32.0372948293931,7.46288180360713));
#7952=CARTESIAN_POINT('Ctrl Pts',(40.8127049623631,-32.5284242284091,7.40995356386524));
#7953=CARTESIAN_POINT('Ctrl Pts',(39.8718186484578,-32.652732185038,7.35702532412334));
#7954=CARTESIAN_POINT('Ctrl Pts',(39.0940512938662,-32.3533177392424,7.30409708438145));
#7955=CARTESIAN_POINT('Ctrl Pts',(38.3162839392746,-32.0539032934467,7.25116884463955));
#7956=CARTESIAN_POINT('Ctrl Pts',(37.7016355439968,-31.3307664452267,7.19824060489766));
#7957=CARTESIAN_POINT('Ctrl Pts',(37.531456342157,-30.514917123868,7.14531236515576));
#7958=CARTESIAN_POINT('Ctrl Pts',(37.4963786231659,-30.34675243086,7.13440267760117));
#7959=CARTESIAN_POINT('Ctrl Pts',(37.4801847910183,-30.1746487205307,7.12349299004658));
#7960=CARTESIAN_POINT('Ctrl Pts',(37.4817753207913,-30.0022480736136,7.11258330249199));
#7961=CARTESIAN_POINT('Ctrl Pts',(37.4864395637057,-30.0006322084003,7.38741669750802));
#7962=CARTESIAN_POINT('Ctrl Pts',(37.4855830611354,-30.3818237963733,7.41142596246837));
#7963=CARTESIAN_POINT('Ctrl Pts',(37.5668725783754,-30.7626687182516,7.43543522742872));
#7964=CARTESIAN_POINT('Ctrl Pts',(37.7321838068588,-31.1026604798972,7.45944449238906));
#7965=CARTESIAN_POINT('Ctrl Pts',(38.0966111372102,-31.8521697006237,7.51237273213096));
#7966=CARTESIAN_POINT('Ctrl Pts',(38.8693660289545,-32.4031412928472,7.56530097187285));
#7967=CARTESIAN_POINT('Ctrl Pts',(39.696726328624,-32.5033727596101,7.61822921161475));
#7968=CARTESIAN_POINT('Ctrl Pts',(40.5240866282935,-32.603604226373,7.67115745135664));
#7969=CARTESIAN_POINT('Ctrl Pts',(41.4060523358881,-32.2530955676754,7.72408569109853));
#7970=CARTESIAN_POINT('Ctrl Pts',(41.9389109023006,-31.6122888303354,7.77701393084043));
#7971=CARTESIAN_POINT('Ctrl Pts',(42.4717694687131,-30.9714820929955,7.82994217058232));
#7972=CARTESIAN_POINT('Ctrl Pts',(42.6555208939435,-30.0403772770133,7.88287041032422));
#7973=CARTESIAN_POINT('Ctrl Pts',(42.40605454299,-29.2451807135995,7.93579865006611));
#7974=CARTESIAN_POINT('Ctrl Pts',(42.1565881920366,-28.4499841501856,7.98872688980801));
#7975=CARTESIAN_POINT('Ctrl Pts',(41.4739040648993,-27.7906958393402,8.0416551295499));
#7976=CARTESIAN_POINT('Ctrl Pts',(40.6704950578746,-27.569097977497,8.09458336929179));
#7977=CARTESIAN_POINT('Ctrl Pts',(39.8670860508498,-27.3475001156537,8.14751160903369));
#7978=CARTESIAN_POINT('Ctrl Pts',(38.9429521639374,-27.5635927028126,8.20043984877559));
#7979=CARTESIAN_POINT('Ctrl Pts',(38.3211082989912,-28.1184643026878,8.25336808851748));
#7980=CARTESIAN_POINT('Ctrl Pts',(37.7961377255517,-28.5868958148278,8.298050958181));
#7981=CARTESIAN_POINT('Ctrl Pts',(37.4866094758723,-29.2967753816077,8.34273382784451));
#7982=CARTESIAN_POINT('Ctrl Pts',(37.4805319060517,-30.0019779656107,8.38741669750802));
#7983=CARTESIAN_POINT('Origin',(40.,-30.,5.));
#7984=CARTESIAN_POINT('',(37.4802181636634,-29.9981833349058,9.38741669750803));
#7985=CARTESIAN_POINT('',(37.4857778982365,-29.998587099551,9.11258330249199));
#7986=CARTESIAN_POINT('',(37.4825,-30.,5.));
#7987=CARTESIAN_POINT('',(41.9134659966651,-28.3640127966251,10.));
#7988=CARTESIAN_POINT('Ctrl Pts',(37.4802181636634,-29.9981833349058,9.38741669750803));
#7989=CARTESIAN_POINT('Ctrl Pts',(37.4861414700995,-30.7144624754953,9.43282641244634));
#7990=CARTESIAN_POINT('Ctrl Pts',(37.8070289114727,-31.4352475048581,9.47823612738464));
#7991=CARTESIAN_POINT('Ctrl Pts',(38.3470252274242,-31.904137664027,9.52364584232294));
#7992=CARTESIAN_POINT('Ctrl Pts',(38.9764291888727,-32.4506623623392,9.57657408206484));
#7993=CARTESIAN_POINT('Ctrl Pts',(39.9035046931223,-32.6549739267535,9.62950232180674));
#7994=CARTESIAN_POINT('Ctrl Pts',(40.7037783386841,-32.421913350571,9.68243056154863));
#7995=CARTESIAN_POINT('Ctrl Pts',(41.5040519842458,-32.1888527743885,9.73535880129053));
#7996=CARTESIAN_POINT('Ctrl Pts',(42.1775237711198,-31.5184200576092,9.78828704103242));
#7997=CARTESIAN_POINT('Ctrl Pts',(42.4158924070768,-30.7212946398739,9.84121528077432));
#7998=CARTESIAN_POINT('Ctrl Pts',(42.6542610430338,-29.9241692221385,9.89414352051621));
#7999=CARTESIAN_POINT('Ctrl Pts',(42.4575265280738,-29.0003511034471,9.94707176025811));
#8000=CARTESIAN_POINT('Ctrl Pts',(41.9134659966651,-28.364012796625,10.));
#8001=CARTESIAN_POINT('',(38.0828940514472,-28.3612424815972,10.));
#8002=CARTESIAN_POINT('Origin',(40.,-30.,10.));
#8003=CARTESIAN_POINT('Ctrl Pts',(38.0828911169303,-28.3612402481786,10.));
#8004=CARTESIAN_POINT('Ctrl Pts',(38.6136994556452,-27.7421357853924,9.94821753066413));
#8005=CARTESIAN_POINT('Ctrl Pts',(39.4733001098964,-27.4026442541442,9.89643506132826));
#8006=CARTESIAN_POINT('Ctrl Pts',(40.2836370984124,-27.4944841015763,9.84465259199238));
#8007=CARTESIAN_POINT('Ctrl Pts',(41.1119040959113,-27.5883560533215,9.79172435225049));
#8008=CARTESIAN_POINT('Ctrl Pts',(41.8887032331835,-28.1328583586548,9.7387961125086));
#8009=CARTESIAN_POINT('Ctrl Pts',(42.2589671420342,-28.8793789236736,9.6858678727667));
#8010=CARTESIAN_POINT('Ctrl Pts',(42.629231050885,-29.6258994886923,9.6329396330248));
#8011=CARTESIAN_POINT('Ctrl Pts',(42.5929597313141,-30.5744383133966,9.58001139328291));
#8012=CARTESIAN_POINT('Ctrl Pts',(42.1665029498384,-31.2904957212721,9.52708315354101));
#8013=CARTESIAN_POINT('Ctrl Pts',(41.7400461683628,-32.0065531291476,9.47415491379912));
#8014=CARTESIAN_POINT('Ctrl Pts',(40.9234039249823,-32.4901291201944,9.42122667405723));
#8015=CARTESIAN_POINT('Ctrl Pts',(40.0905142258871,-32.5200278866053,9.36829843431534));
#8016=CARTESIAN_POINT('Ctrl Pts',(39.2576245267919,-32.5499266530163,9.31537019457344));
#8017=CARTESIAN_POINT('Ctrl Pts',(38.408487371982,-32.1261481947915,9.26244195483155));
#8018=CARTESIAN_POINT('Ctrl Pts',(37.9317247877119,-31.4425949153635,9.20951371508965));
#8019=CARTESIAN_POINT('Ctrl Pts',(37.640684225183,-31.02531860735,9.17720357755709));
#8020=CARTESIAN_POINT('Ctrl Pts',(37.4884095532307,-30.5112368586177,9.14489344002454));
#8021=CARTESIAN_POINT('Ctrl Pts',(37.4857778982365,-29.998587099551,9.11258330249199));
#8022=CARTESIAN_POINT('Origin',(40.,30.,12.2084234471775));
#8023=CARTESIAN_POINT('',(36.9214104210795,30.0001481134795,0.791576552822544));
#8024=CARTESIAN_POINT('',(36.9314435342158,30.0007393170824,0.708423447177453));
#8025=CARTESIAN_POINT('',(36.9265,30.0000000000001,12.2084234471775));
#8026=CARTESIAN_POINT('',(40.7937992825328,27.0307770462543,0.));
#8027=CARTESIAN_POINT('Ctrl Pts',(36.9314435342158,30.0007393170824,0.708423447177453));
#8028=CARTESIAN_POINT('Ctrl Pts',(36.9305908971901,30.4743000521285,0.68399525708588));
#8029=CARTESIAN_POINT('Ctrl Pts',(37.2564683870193,31.9726985654157,0.606638827252413));
#8030=CARTESIAN_POINT('Ctrl Pts',(39.5908855572201,33.609027296031,0.47635415767705));
#8031=CARTESIAN_POINT('Ctrl Pts',(42.8129709591412,32.3023681766822,0.317569438451369));
#8032=CARTESIAN_POINT('Ctrl Pts',(43.4548287867864,28.8815849473274,0.158784719225683));
#8033=CARTESIAN_POINT('Ctrl Pts',(41.7812379463276,27.2947612990625,0.0529282397418946));
#8034=CARTESIAN_POINT('Ctrl Pts',(40.7937992825328,27.0307770462543,0.));
#8035=CARTESIAN_POINT('',(39.2062007174671,27.0307770462543,0.));
#8036=CARTESIAN_POINT('Origin',(40.,30.,0.));
#8037=CARTESIAN_POINT('Ctrl Pts',(36.9214104210795,30.0001481134795,0.791576552822544));
#8038=CARTESIAN_POINT('Ctrl Pts',(36.9214060852395,30.0071343339544,0.791213130185148));
#8039=CARTESIAN_POINT('Ctrl Pts',(36.9245904926899,31.0315771191332,0.737921467805857));
#8040=CARTESIAN_POINT('Ctrl Pts',(38.0509704657541,33.0656996094815,0.631701565684668));
#8041=CARTESIAN_POINT('Ctrl Pts',(41.5191020833988,33.300338163167,0.472916846458987));
#8042=CARTESIAN_POINT('Ctrl Pts',(43.5964449208384,30.5125900673602,0.314132127233303));
#8043=CARTESIAN_POINT('Ctrl Pts',(42.3902201567819,27.281023587038,0.15649317841364));
#8044=CARTESIAN_POINT('Ctrl Pts',(40.1666400375141,26.7696589897829,0.0517824693358737));
#8045=CARTESIAN_POINT('Ctrl Pts',(39.2044526546617,27.0254683880106,-4.06575814682064E-18));
#8046=CARTESIAN_POINT('Origin',(40.,30.,12.2084234471775));
#8047=CARTESIAN_POINT('',(36.9285654760686,30.0025993155776,1.79157655282254));
#8048=CARTESIAN_POINT('',(36.9266847216198,29.9971878060927,1.70842344717745));
#8049=CARTESIAN_POINT('',(36.9265,30.0000000000001,12.2084234471775));
#8050=CARTESIAN_POINT('Ctrl Pts',(36.9266847216198,29.9971878060927,1.70842344717745));
#8051=CARTESIAN_POINT('Ctrl Pts',(36.9337736898222,30.7732902078871,1.66823136220391));
#8052=CARTESIAN_POINT('Ctrl Pts',(37.6258961169519,32.5826850742956,1.57511103748848));
#8053=CARTESIAN_POINT('Ctrl Pts',(40.6663949910499,33.5712523754168,1.42906247303115));
#8054=CARTESIAN_POINT('Ctrl Pts',(43.3620055739433,31.3766529896116,1.27027775380547));
#8055=CARTESIAN_POINT('Ctrl Pts',(42.9796780358998,27.9216547954996,1.11149303457979));
#8056=CARTESIAN_POINT('Ctrl Pts',(39.8696594013047,26.3695385472464,0.952708315354102));
#8057=CARTESIAN_POINT('Ctrl Pts',(37.3388060344315,27.8681888840249,0.81835178621999));
#8058=CARTESIAN_POINT('Ctrl Pts',(36.9324382946739,29.448242205726,0.736923496827775));
#8059=CARTESIAN_POINT('Ctrl Pts',(36.9314435342158,30.0007393170824,0.708423447177453));
#8060=CARTESIAN_POINT('Ctrl Pts',(36.9285654760686,30.0025993155776,1.79157655282254));
#8061=CARTESIAN_POINT('Ctrl Pts',(36.9260623773303,30.3144991191654,1.77544923530318));
#8062=CARTESIAN_POINT('Ctrl Pts',(37.1131652421759,31.6470901191891,1.70639367804192));
#8063=CARTESIAN_POINT('Ctrl Pts',(39.0340361139851,33.5021320828999,1.58440988103877));
#8064=CARTESIAN_POINT('Ctrl Pts',(42.4187332816925,32.7106797239938,1.42562516181309));
#8065=CARTESIAN_POINT('Ctrl Pts',(43.5891188868934,29.4376293695436,1.2668404425874));
#8066=CARTESIAN_POINT('Ctrl Pts',(41.4737278337939,26.6794509596774,1.10805572336172));
#8067=CARTESIAN_POINT('Ctrl Pts',(38.0170881375389,26.9604739257629,0.949634426773431));
#8068=CARTESIAN_POINT('Ctrl Pts',(36.9220375494226,28.9896733556398,0.844141369927042));
#8069=CARTESIAN_POINT('Ctrl Pts',(36.9214104210795,30.0001481134795,0.791576552822544));
#8070=CARTESIAN_POINT('Origin',(40.,30.,12.2084234471775));
#8071=CARTESIAN_POINT('',(36.9306301640296,29.9983760595424,2.79157655282254));
#8072=CARTESIAN_POINT('',(36.9218442521368,30.001056467914,2.70842344717745));
#8073=CARTESIAN_POINT('',(36.9265,30.0000000000001,12.2084234471775));
#8074=CARTESIAN_POINT('Ctrl Pts',(36.9218442521368,30.001056467914,2.70842344717745));
#8075=CARTESIAN_POINT('Ctrl Pts',(36.9215847759613,30.0592829556301,2.70539570706384));
#8076=CARTESIAN_POINT('Ctrl Pts',(36.9494734222224,31.1351192558441,2.64943972720834));
#8077=CARTESIAN_POINT('Ctrl Pts',(38.2073434453337,33.1598130705237,2.54055550761094));
#8078=CARTESIAN_POINT('Ctrl Pts',(41.6828293076519,33.2196458493402,2.38177078838525));
#8079=CARTESIAN_POINT('Ctrl Pts',(43.6177133488499,30.3319467933355,2.22298606915957));
#8080=CARTESIAN_POINT('Ctrl Pts',(42.2406393602062,27.1403544247083,2.06420134993389));
#8081=CARTESIAN_POINT('Ctrl Pts',(38.8122994891743,26.5667233512227,1.9054166307082));
#8082=CARTESIAN_POINT('Ctrl Pts',(37.0638424029061,28.4858017899762,1.78682399645606));
#8083=CARTESIAN_POINT('Ctrl Pts',(36.9244383540519,29.7512547993364,1.72115960194581));
#8084=CARTESIAN_POINT('Ctrl Pts',(36.9266847216198,29.9971878060927,1.70842344717745));
#8085=CARTESIAN_POINT('Ctrl Pts',(36.9306301640296,29.9983760595424,2.79157655282254));
#8086=CARTESIAN_POINT('Ctrl Pts',(36.9335903506277,30.61619128252,2.75968534042121));
#8087=CARTESIAN_POINT('Ctrl Pts',(37.4143806753803,32.2636022177905,2.67486588827799));
#8088=CARTESIAN_POINT('Ctrl Pts',(40.1017542133218,33.6314839980979,2.53711819639287));
#8089=CARTESIAN_POINT('Ctrl Pts',(43.1063930447263,31.883707179614,2.37833347716719));
#8090=CARTESIAN_POINT('Ctrl Pts',(43.2671803398556,28.4114273111418,2.21954875794151));
#8091=CARTESIAN_POINT('Ctrl Pts',(40.4369180427711,26.3934599853152,2.06076403871582));
#8092=CARTESIAN_POINT('Ctrl Pts',(37.5347521985174,27.5468316477252,1.9181066370095));
#8093=CARTESIAN_POINT('Ctrl Pts',(36.9342772965169,29.2908752238756,1.82837747504508));
#8094=CARTESIAN_POINT('Ctrl Pts',(36.9285654760686,30.0025993155776,1.79157655282254));
#8095=CARTESIAN_POINT('Origin',(40.,30.,12.2084234471775));
#8096=CARTESIAN_POINT('',(36.9226404245075,29.9982621359517,3.79157655282254));
#8097=CARTESIAN_POINT('',(36.9298121415154,30.0021532465789,3.70842344717745));
#8098=CARTESIAN_POINT('',(36.9265,30.0000000000001,12.2084234471775));
#8099=CARTESIAN_POINT('Ctrl Pts',(36.9298121415154,30.0021532465789,3.70842344717745));
#8100=CARTESIAN_POINT('Ctrl Pts',(36.9274611424663,30.3659528285612,3.68963181218188));
#8101=CARTESIAN_POINT('Ctrl Pts',(37.1555525490304,31.7515729915281,3.61791193744441));
#8102=CARTESIAN_POINT('Ctrl Pts',(39.2110614856976,33.5462109122232,3.49326382296504));
#8103=CARTESIAN_POINT('Ctrl Pts',(42.551760057577,32.5858376556528,3.33447910373935));
#8104=CARTESIAN_POINT('Ctrl Pts',(43.5563644593613,29.2581727531378,3.17569438451367));
#8105=CARTESIAN_POINT('Ctrl Pts',(41.3051759276346,26.6096384170271,3.01690966528799));
#8106=CARTESIAN_POINT('Ctrl Pts',(37.9248305372375,27.0562426682318,2.86115268617592));
#8107=CARTESIAN_POINT('Ctrl Pts',(36.9261207059647,29.0414196696403,2.75832394680574));
#8108=CARTESIAN_POINT('Ctrl Pts',(36.9218442521368,30.001056467914,2.70842344717745));
#8109=CARTESIAN_POINT('Ctrl Pts',(36.9226404245075,29.9982621359517,3.79157655282254));
#8110=CARTESIAN_POINT('Ctrl Pts',(36.9288449239179,30.91534466323,3.74392144553925));
#8111=CARTESIAN_POINT('Ctrl Pts',(37.8505480972411,32.8618102457237,3.64333809851406));
#8112=CARTESIAN_POINT('Ctrl Pts',(41.1605538126502,33.4425492067914,3.48982651174697));
#8113=CARTESIAN_POINT('Ctrl Pts',(43.5217905842841,30.8916396581577,3.33104179252129));
#8114=CARTESIAN_POINT('Ctrl Pts',(42.6588862528215,27.5244487277861,3.17225707329561));
#8115=CARTESIAN_POINT('Ctrl Pts',(39.3618154801332,26.4235841007334,3.01347235406992));
#8116=CARTESIAN_POINT('Ctrl Pts',(37.1938507363835,28.1603743953028,2.88657884724557));
#8117=CARTESIAN_POINT('Ctrl Pts',(36.9286774779537,29.5908344592533,2.81261358016311));
#8118=CARTESIAN_POINT('Ctrl Pts',(36.9306301640296,29.9983760595424,2.79157655282254));
#8119=CARTESIAN_POINT('Origin',(40.,30.,12.2084234471775));
#8120=CARTESIAN_POINT('',(36.9253702239752,30.0027105193813,4.79157655282255));
#8121=CARTESIAN_POINT('',(36.9296341594976,29.9977623726118,4.70842344717745));
#8122=CARTESIAN_POINT('',(36.9265,30.0000000000001,12.2084234471775));
#8123=CARTESIAN_POINT('Ctrl Pts',(36.9296341594976,29.9977623726118,4.70842344717745));
#8124=CARTESIAN_POINT('Ctrl Pts',(36.9341435373618,30.6666480454017,4.67386791729991));
#8125=CARTESIAN_POINT('Ctrl Pts',(37.4780313316422,32.3667321797224,4.58638414768047));
#8126=CARTESIAN_POINT('Ctrl Pts',(40.2839268182445,33.6217980846202,4.44597213831914));
#8127=CARTESIAN_POINT('Ctrl Pts',(43.1970393894843,31.7253912441272,4.28718741909346));
#8128=CARTESIAN_POINT('Ctrl Pts',(43.1833152122909,28.2494172218816,4.12840269986777));
#8129=CARTESIAN_POINT('Ctrl Pts',(40.255318543719,26.3760728144276,3.96961798064209));
#8130=CARTESIAN_POINT('Ctrl Pts',(37.4677628071963,27.6494457306752,3.82962489641198));
#8131=CARTESIAN_POINT('Ctrl Pts',(36.9340829314343,29.3412803347791,3.74256005192377));
#8132=CARTESIAN_POINT('Ctrl Pts',(36.9298121415154,30.0021532465789,3.70842344717745));
#8133=CARTESIAN_POINT('Ctrl Pts',(36.9253702239752,30.0027105193813,4.79157655282255));
#8134=CARTESIAN_POINT('Ctrl Pts',(36.9235103917928,30.2050629564242,4.78108579039918));
#8135=CARTESIAN_POINT('Ctrl Pts',(37.0339430833948,31.4263085444825,4.71766678823391));
#8136=CARTESIAN_POINT('Ctrl Pts',(38.6680931462871,33.3799488650141,4.60131954632676));
#8137=CARTESIAN_POINT('Ctrl Pts',(42.1176356506926,32.9518891320487,4.44253482710108));
#8138=CARTESIAN_POINT('Ctrl Pts',(43.6285176985082,29.8214236615297,4.28375010787539));
#8139=CARTESIAN_POINT('Ctrl Pts',(41.8175517334939,26.8544418788833,4.1249653886497));
#8140=CARTESIAN_POINT('Ctrl Pts',(38.3426471809504,26.7671665941811,3.96618066942403));
#8141=CARTESIAN_POINT('Ctrl Pts',(36.9725521563655,28.7774415912537,3.85505105748164));
#8142=CARTESIAN_POINT('Ctrl Pts',(36.9219538843002,29.8967851292364,3.79684968528114));
#8143=CARTESIAN_POINT('Ctrl Pts',(36.9226404245075,29.9982621359517,3.79157655282254));
#8144=CARTESIAN_POINT('Origin',(40.,30.,12.2084234471775));
#8145=CARTESIAN_POINT('',(36.9314878993762,30.0000666771347,5.79157655282255));
#8146=CARTESIAN_POINT('',(36.9217350264198,29.9990828880962,5.70842344717746));
#8147=CARTESIAN_POINT('',(36.9265,30.0000000000001,12.2084234471775));
#8148=CARTESIAN_POINT('Ctrl Pts',(36.9217350264198,29.9990828880962,5.70842344717746));
#8149=CARTESIAN_POINT('Ctrl Pts',(36.925541226593,30.966684508532,5.65810402241795));
#8150=CARTESIAN_POINT('Ctrl Pts',(37.9390395048434,32.9589227335458,5.55485635791654));
#8151=CARTESIAN_POINT('Ctrl Pts',(41.3319071366153,33.3799495829286,5.39868045367324));
#8152=CARTESIAN_POINT('Ctrl Pts',(43.562111392168,30.7137213976436,5.23989573444756));
#8153=CARTESIAN_POINT('Ctrl Pts',(42.5312615113734,27.3940930629228,5.08111101522188));
#8154=CARTESIAN_POINT('Ctrl Pts',(39.1830835312918,26.4601294816251,4.92232629599619));
#8155=CARTESIAN_POINT('Ctrl Pts',(37.1486704266839,28.2648568201031,4.79809710664805));
#8156=CARTESIAN_POINT('Ctrl Pts',(36.9272365840166,29.6421248685093,4.7267961570418));
#8157=CARTESIAN_POINT('Ctrl Pts',(36.9296341594976,29.9977623726118,4.70842344717745));
#8158=CARTESIAN_POINT('Ctrl Pts',(36.9314878993762,30.0000666771347,5.79157655282255));
#8159=CARTESIAN_POINT('Ctrl Pts',(36.9313894343278,30.5090425915801,5.76532189551722));
#8160=CARTESIAN_POINT('Ctrl Pts',(37.2923228112074,32.0439602821561,5.68613899846999));
#8161=CARTESIAN_POINT('Ctrl Pts',(39.7160732420625,33.6217973153363,5.55402786168086));
#8162=CARTESIAN_POINT('Ctrl Pts',(42.8891154512744,32.2025081398842,5.39524314245518));
#8163=CARTESIAN_POINT('Ctrl Pts',(43.4172201906419,28.7668591460577,5.23645842322949));
#8164=CARTESIAN_POINT('Ctrl Pts',(40.8169162951919,26.4601302335076,5.07767370400381));
#8165=CARTESIAN_POINT('Ctrl Pts',(37.6899500625198,27.3323875025768,4.92937974720149));
#8166=CARTESIAN_POINT('Ctrl Pts',(36.9328936605827,29.1841497121866,4.83401403014107));
#8167=CARTESIAN_POINT('Ctrl Pts',(36.9253702239752,30.0027105193813,4.79157655282255));
#8168=CARTESIAN_POINT('Origin',(40.,30.,12.2084234471775));
#8169=CARTESIAN_POINT('',(36.9256150573553,29.9972554300884,6.79157655282254));
#8170=CARTESIAN_POINT('',(36.926927637137,30.0028093909042,6.70842344717746));
#8171=CARTESIAN_POINT('',(36.9265,30.0000000000001,12.2084234471775));
#8172=CARTESIAN_POINT('Ctrl Pts',(36.926927637137,30.0028093909042,6.70842344717746));
#8173=CARTESIAN_POINT('Ctrl Pts',(36.9246261470968,30.2568826318381,6.69526836727787));
#8174=CARTESIAN_POINT('Ctrl Pts',(37.0696627317,31.5306040707075,6.6291850476364));
#8175=CARTESIAN_POINT('Ctrl Pts',(38.8394459408439,33.4425499380084,6.51017348825303));
#8176=CARTESIAN_POINT('Ctrl Pts',(42.2631512836135,32.8418624302693,6.35138876902734));
#8177=CARTESIAN_POINT('Ctrl Pts',(43.6149790117272,29.6394968119162,6.19260404980166));
#8178=CARTESIAN_POINT('Ctrl Pts',(41.657353171078,26.7671659075135,6.03381933057598));
#8179=CARTESIAN_POINT('Ctrl Pts',(38.1824478804507,26.8544412107546,5.87503461135029));
#8180=CARTESIAN_POINT('Ctrl Pts',(36.9453830083193,28.8811766715375,5.76656931688412));
#8181=CARTESIAN_POINT('Ctrl Pts',(36.9215376936385,29.9489174973662,5.71103226215984));
#8182=CARTESIAN_POINT('Ctrl Pts',(36.9217350264198,29.9990828880962,5.70842344717746));
#8183=CARTESIAN_POINT('Ctrl Pts',(36.9256150573553,29.9972554300884,6.79157655282254));
#8184=CARTESIAN_POINT('Ctrl Pts',(36.9330938990886,30.8079017788323,6.74955800063525));
#8185=CARTESIAN_POINT('Ctrl Pts',(37.6777711979151,32.6518218559865,6.65461120870606));
#8186=CARTESIAN_POINT('Ctrl Pts',(40.7889383467181,33.5462101590121,6.50673617703496));
#8187=CARTESIAN_POINT('Ctrl Pts',(43.4073761900399,31.2600863855708,6.34795145780928));
#8188=CARTESIAN_POINT('Ctrl Pts',(42.9064174160314,27.8203743447495,6.1891667385836));
#8189=CARTESIAN_POINT('Ctrl Pts',(39.7446815105131,26.3760735841615,6.03038201935791));
#8190=CARTESIAN_POINT('Ctrl Pts',(37.3008223075735,27.9396648339668,5.89785195743756));
#8191=CARTESIAN_POINT('Ctrl Pts',(36.9315879355548,29.4829694301855,5.81825013525911));
#8192=CARTESIAN_POINT('Ctrl Pts',(36.9314878993762,30.0000666771347,5.79157655282255));
#8193=CARTESIAN_POINT('Origin',(40.,30.,12.2084234471775));
#8194=CARTESIAN_POINT('',(36.9224678986813,30.0016204990256,7.79157655282255));
#8195=CARTESIAN_POINT('',(36.9313094744419,29.9992281658451,7.70842344717746));
#8196=CARTESIAN_POINT('',(36.9265,30.0000000000001,12.2084234471775));
#8197=CARTESIAN_POINT('Ctrl Pts',(36.9313094744419,29.9992281658452,7.70842344717746));
#8198=CARTESIAN_POINT('Ctrl Pts',(36.9325689694722,30.5597739580728,7.67950447239591));
#8199=CARTESIAN_POINT('Ctrl Pts',(37.347926997611,32.1479826672757,7.59765725787247));
#8200=CARTESIAN_POINT('Ctrl Pts',(39.8982457650928,33.6314847697161,7.46288180360713));
#8201=CARTESIAN_POINT('Ctrl Pts',(42.9960395463676,32.0546977641436,7.30409708438144));
#8202=CARTESIAN_POINT('Ctrl Pts',(43.3510086198694,28.5968688366528,7.14531236515576));
#8203=CARTESIAN_POINT('Ctrl Pts',(40.6381846554167,26.4235833410482,6.98652764593007));
#8204=CARTESIAN_POINT('Ctrl Pts',(37.6142706932541,27.4332431712104,6.84089800660398));
#8205=CARTESIAN_POINT('Ctrl Pts',(36.933885978093,29.2346425914276,6.74819660701977));
#8206=CARTESIAN_POINT('Ctrl Pts',(36.926927637137,30.0028093909042,6.70842344717746));
#8207=CARTESIAN_POINT('Ctrl Pts',(36.9224678986813,30.0016204990256,7.79157655282255));
#8208=CARTESIAN_POINT('Ctrl Pts',(36.9218704635921,30.0950218610504,7.78672234549518));
#8209=CARTESIAN_POINT('Ctrl Pts',(36.9680973053051,31.2062330488769,7.72893989842591));
#8210=CARTESIAN_POINT('Ctrl Pts',(38.3171710506372,33.2196451638042,7.61822921161474));
#8211=CARTESIAN_POINT('Ctrl Pts',(41.7926561734374,33.159812400248,7.45944449238906));
#8212=CARTESIAN_POINT('Ctrl Pts',(43.6269944901785,30.207223201086,7.30065977316338));
#8213=CARTESIAN_POINT('Ctrl Pts',(42.1408791121553,27.0649247751536,7.14187505393769));
#8214=CARTESIAN_POINT('Ctrl Pts',(38.6948243496615,26.6096391370258,6.98309033471202));
#8215=CARTESIAN_POINT('Ctrl Pts',(37.0393590026679,28.5573022279082,6.86632416767362));
#8216=CARTESIAN_POINT('Ctrl Pts',(36.9236732525493,29.7867793922029,6.80248624037714));
#8217=CARTESIAN_POINT('Ctrl Pts',(36.9256150573553,29.9972554300884,6.79157655282254));
#8218=CARTESIAN_POINT('Origin',(40.,30.,12.2084234471775));
#8219=CARTESIAN_POINT('',(36.9305016190506,30.0017249535699,8.79157655282255));
#8220=CARTESIAN_POINT('',(36.9240970871575,29.9975851957844,8.70842344717746));
#8221=CARTESIAN_POINT('',(36.9265,30.0000000000001,12.2084234471775));
#8222=CARTESIAN_POINT('Ctrl Pts',(36.9240970871575,29.9975851957844,8.70842344717746));
#8223=CARTESIAN_POINT('Ctrl Pts',(36.9315169131983,30.8585346510502,8.66374057751394));
#8224=CARTESIAN_POINT('Ctrl Pts',(37.7570267321285,32.7517788120336,8.56612946810854));
#8225=CARTESIAN_POINT('Ctrl Pts',(40.9659640933653,33.5021328388261,8.41559011896122));
#8226=CARTESIAN_POINT('Ctrl Pts',(43.4663372079312,31.0874483526599,8.25680539973555));
#8227=CARTESIAN_POINT('Ctrl Pts',(42.7933361741705,27.6772190016871,8.09802068050986));
#8228=CARTESIAN_POINT('Ctrl Pts',(39.5630818641794,26.3934592174139,7.93923596128418));
#8229=CARTESIAN_POINT('Ctrl Pts',(37.2482860828349,28.0439006852296,7.80937021684004));
#8230=CARTESIAN_POINT('Ctrl Pts',(36.930263809783,29.5338488586718,7.7324327121378));
#8231=CARTESIAN_POINT('Ctrl Pts',(36.9313094744419,29.9992281658452,7.70842344717746));
#8232=CARTESIAN_POINT('Ctrl Pts',(36.9305016190507,30.0017249535699,8.79157655282255));
#8233=CARTESIAN_POINT('Ctrl Pts',(36.9284513914002,30.4011123899437,8.77095845061321));
#8234=CARTESIAN_POINT('Ctrl Pts',(37.1865084098534,31.8232183849388,8.69741210866198));
#8235=CARTESIAN_POINT('Ctrl Pts',(39.3336051768584,33.5712515449036,8.57093752696884));
#8236=CARTESIAN_POINT('Ctrl Pts',(42.63924979695,32.4964766410994,8.41215280774317));
#8237=CARTESIAN_POINT('Ctrl Pts',(43.5287243142158,29.1361944846783,8.25336808851748));
#8238=CARTESIAN_POINT('Ctrl Pts',(41.1877002535156,26.5667240916348,8.0945833692918));
#8239=CARTESIAN_POINT('Ctrl Pts',(37.864168867224,27.12281855603,7.94065285739348));
#8240=CARTESIAN_POINT('Ctrl Pts',(36.9283846451053,29.0766126032515,7.83965058523707));
#8241=CARTESIAN_POINT('Ctrl Pts',(36.9224678986813,30.0016204990256,7.79157655282255));
#8242=CARTESIAN_POINT('Origin',(40.,30.,12.2084234471775));
#8243=CARTESIAN_POINT('',(36.9295987310864,29.9965353802945,9.79157655282255));
#8244=CARTESIAN_POINT('',(36.9237140680981,30.0022179367619,9.70842344717746));
#8245=CARTESIAN_POINT('',(36.9265,30.0000000000001,12.2084234471775));
#8246=CARTESIAN_POINT('',(39.2062007174671,27.0307770462543,10.));
#8247=CARTESIAN_POINT('Ctrl Pts',(39.2062007174671,27.0307770462543,10.));
#8248=CARTESIAN_POINT('Ctrl Pts',(38.2187620536724,27.2947612990625,9.94707176025811));
#8249=CARTESIAN_POINT('Ctrl Pts',(37.1203696025755,28.3362007046644,9.87759727786562));
#8250=CARTESIAN_POINT('Ctrl Pts',(36.9271780976658,29.6764519122675,9.80812279547314));
#8251=CARTESIAN_POINT('Ctrl Pts',(36.9295987310864,29.9965353802945,9.79157655282255));
#8252=CARTESIAN_POINT('',(40.7955467101491,27.0254727950732,10.));
#8253=CARTESIAN_POINT('Origin',(40.,30.,10.));
#8254=CARTESIAN_POINT('Ctrl Pts',(40.7955481281091,27.0254684909089,10.));
#8255=CARTESIAN_POINT('Ctrl Pts',(39.8333613752542,26.7696596878221,9.94821753066413));
#8256=CARTESIAN_POINT('Ctrl Pts',(37.7694374933144,27.2443038752448,9.85102534638994));
#8257=CARTESIAN_POINT('Ctrl Pts',(36.9309454989351,29.1277455385835,9.75383316211576));
#8258=CARTESIAN_POINT('Ctrl Pts',(36.9237140680981,30.0022179367619,9.70842344717746));
#8259=CARTESIAN_POINT('Origin',(-40.,30.,12.2084234471774));
#8260=CARTESIAN_POINT('',(-43.0785897715144,30.0001480928245,0.791576552822542));
#8261=CARTESIAN_POINT('',(-43.0685559416288,30.0007395458647,0.708423447177451));
#8262=CARTESIAN_POINT('',(-43.0735,30.0000000000001,12.2084234471774));
#8263=CARTESIAN_POINT('',(-39.2062007174671,27.0307770462543,0.));
#8264=CARTESIAN_POINT('Ctrl Pts',(-43.0685559416287,30.0007395458647,0.708423447177451));
#8265=CARTESIAN_POINT('Ctrl Pts',(-43.0694085603479,30.4743003164273,0.683995257085879));
#8266=CARTESIAN_POINT('Ctrl Pts',(-42.7435310628009,31.9726987925452,0.606638827252412));
#8267=CARTESIAN_POINT('Ctrl Pts',(-40.4091143183855,33.6090247272076,0.476354157677051));
#8268=CARTESIAN_POINT('Ctrl Pts',(-37.1870300541988,32.3023712386336,0.317569438451368));
#8269=CARTESIAN_POINT('Ctrl Pts',(-36.5451700500256,28.8815775163836,0.158784719225683));
#8270=CARTESIAN_POINT('Ctrl Pts',(-38.2187620536724,27.2947612990625,0.0529282397418946));
#8271=CARTESIAN_POINT('Ctrl Pts',(-39.2062007174671,27.0307770462543,0.));
#8272=CARTESIAN_POINT('',(-40.7937992825329,27.0307770462543,0.));
#8273=CARTESIAN_POINT('Origin',(-40.,30.,0.));
#8274=CARTESIAN_POINT('Ctrl Pts',(-43.0785897715144,30.0001480928245,0.791576552822542));
#8275=CARTESIAN_POINT('Ctrl Pts',(-43.0785941073969,30.0071343138444,0.791213130185146));
#8276=CARTESIAN_POINT('Ctrl Pts',(-43.0754097060638,31.0315771792942,0.737921467805855));
#8277=CARTESIAN_POINT('Ctrl Pts',(-41.9490297104332,33.065699934597,0.63170156568467));
#8278=CARTESIAN_POINT('Ctrl Pts',(-38.4808977151712,33.3003381572967,0.472916846458986));
#8279=CARTESIAN_POINT('Ctrl Pts',(-36.4035550591505,30.5125904676491,0.314132127233303));
#8280=CARTESIAN_POINT('Ctrl Pts',(-37.6097792569612,27.2810228199895,0.156493178413639));
#8281=CARTESIAN_POINT('Ctrl Pts',(-39.8333603928249,26.7696592028777,0.0517824693358729));
#8282=CARTESIAN_POINT('Ctrl Pts',(-40.7955475841208,27.0254684201926,2.94089839286693E-17));
#8283=CARTESIAN_POINT('Origin',(-40.,30.,12.2084234471774));
#8284=CARTESIAN_POINT('',(-43.0714347220705,30.0025993151568,1.79157655282254));
#8285=CARTESIAN_POINT('',(-43.0733147540399,29.9971878064111,1.70842344717745));
#8286=CARTESIAN_POINT('',(-43.0735,30.0000000000001,12.2084234471774));
#8287=CARTESIAN_POINT('Ctrl Pts',(-43.0733147540399,29.9971878064111,1.70842344717745));
#8288=CARTESIAN_POINT('Ctrl Pts',(-43.0662257847241,30.773290081476,1.66823136220391));
#8289=CARTESIAN_POINT('Ctrl Pts',(-42.3741034680082,32.5826846574708,1.57511103748848));
#8290=CARTESIAN_POINT('Ctrl Pts',(-39.3336051438857,33.5712517079766,1.42906247303115));
#8291=CARTESIAN_POINT('Ctrl Pts',(-36.6379949650665,31.3766528609059,1.27027775380547));
#8292=CARTESIAN_POINT('Ctrl Pts',(-37.0203225278291,27.921654956147,1.11149303457979));
#8293=CARTESIAN_POINT('Ctrl Pts',(-40.1303404958339,26.3695395185102,0.952708315354101));
#8294=CARTESIAN_POINT('Ctrl Pts',(-42.66119358551,27.8681887692102,0.818351786219991));
#8295=CARTESIAN_POINT('Ctrl Pts',(-43.0675612025287,29.4482423930718,0.736923496827774));
#8296=CARTESIAN_POINT('Ctrl Pts',(-43.0685559416287,30.0007395458647,0.708423447177451));
#8297=CARTESIAN_POINT('Ctrl Pts',(-43.0714347220705,30.0025993151568,1.79157655282254));
#8298=CARTESIAN_POINT('Ctrl Pts',(-43.0739378209611,30.3144991388018,1.77544923530318));
#8299=CARTESIAN_POINT('Ctrl Pts',(-42.886834944053,31.6470902248259,1.70639367804192));
#8300=CARTESIAN_POINT('Ctrl Pts',(-40.9659639490253,33.5021323126134,1.58440988103877));
#8301=CARTESIAN_POINT('Ctrl Pts',(-37.5812665608262,32.7106798921575,1.42562516181309));
#8302=CARTESIAN_POINT('Ctrl Pts',(-36.4108808842817,29.4376293456934,1.2668404425874));
#8303=CARTESIAN_POINT('Ctrl Pts',(-38.5262720652766,26.679450722727,1.10805572336172));
#8304=CARTESIAN_POINT('Ctrl Pts',(-41.9829120023514,26.9604737702103,0.949634426773434));
#8305=CARTESIAN_POINT('Ctrl Pts',(-43.0779626370196,28.9896732561604,0.84414136992704));
#8306=CARTESIAN_POINT('Ctrl Pts',(-43.0785897715144,30.0001480928245,0.791576552822542));
#8307=CARTESIAN_POINT('Origin',(-40.,30.,12.2084234471774));
#8308=CARTESIAN_POINT('',(-43.0693700340734,29.9983760594323,2.79157655282254));
#8309=CARTESIAN_POINT('',(-43.0781552224421,30.001056467624,2.70842344717745));
#8310=CARTESIAN_POINT('',(-43.0735,30.0000000000001,12.2084234471774));
#8311=CARTESIAN_POINT('Ctrl Pts',(-43.0781552224421,30.001056467624,2.70842344717745));
#8312=CARTESIAN_POINT('Ctrl Pts',(-43.0784146985717,30.0592829454032,2.70539570706384));
#8313=CARTESIAN_POINT('Ctrl Pts',(-43.0505260570341,31.1351190620316,2.64943972720834));
#8314=CARTESIAN_POINT('Ctrl Pts',(-41.7926562482662,33.15981253181,2.54055550761094));
#8315=CARTESIAN_POINT('Ctrl Pts',(-38.3171709803108,33.2196452983643,2.38177078838525));
#8316=CARTESIAN_POINT('Ctrl Pts',(-36.3822872674944,30.3319467392027,2.22298606915957));
#8317=CARTESIAN_POINT('Ctrl Pts',(-37.7593610245569,27.1403549081105,2.06420134993389));
#8318=CARTESIAN_POINT('Ctrl Pts',(-41.1877003040245,26.566723946295,1.9054166307082));
#8319=CARTESIAN_POINT('Ctrl Pts',(-42.9361571001743,28.485802038215,1.78682399645606));
#8320=CARTESIAN_POINT('Ctrl Pts',(-43.0755611219607,29.7512548398132,1.72115960194581));
#8321=CARTESIAN_POINT('Ctrl Pts',(-43.0733147540399,29.9971878064111,1.70842344717745));
#8322=CARTESIAN_POINT('Ctrl Pts',(-43.0693700340734,29.9983760594323,2.79157655282254));
#8323=CARTESIAN_POINT('Ctrl Pts',(-43.0664098472836,30.6161913222782,2.75968534042121));
#8324=CARTESIAN_POINT('Ctrl Pts',(-42.5856194914985,32.2636023638608,2.67486588827799));
#8325=CARTESIAN_POINT('Ctrl Pts',(-39.8982457801193,33.6314842325659,2.53711819639287));
#8326=CARTESIAN_POINT('Ctrl Pts',(-36.893606754763,31.8837073010328,2.37833347716719));
#8327=CARTESIAN_POINT('Ctrl Pts',(-36.7328194493102,28.4114272089134,2.21954875794151));
#8328=CARTESIAN_POINT('Ctrl Pts',(-39.5630819289538,26.3934597519746,2.06076403871582));
#8329=CARTESIAN_POINT('Ctrl Pts',(-42.4652479607273,27.5468314902893,1.9181066370095));
#8330=CARTESIAN_POINT('Ctrl Pts',(-43.0657229012746,29.2908751776861,1.82837747504507));
#8331=CARTESIAN_POINT('Ctrl Pts',(-43.0714347220705,30.0025993151568,1.79157655282254));
#8332=CARTESIAN_POINT('Origin',(-40.,30.,12.2084234471774));
#8333=CARTESIAN_POINT('',(-43.0773597741118,29.9982621358397,3.79157655282254));
#8334=CARTESIAN_POINT('',(-43.0701873343651,30.0021532462092,3.70842344717745));
#8335=CARTESIAN_POINT('',(-43.0735,30.0000000000001,12.2084234471774));
#8336=CARTESIAN_POINT('Ctrl Pts',(-43.0701873343651,30.0021532462092,3.70842344717745));
#8337=CARTESIAN_POINT('Ctrl Pts',(-43.0725383330132,30.3659527660857,3.68963181218187));
#8338=CARTESIAN_POINT('Ctrl Pts',(-42.8444469653874,31.7515726925092,3.6179119374444));
#8339=CARTESIAN_POINT('Ctrl Pts',(-40.7889383796118,33.5462103068538,3.49326382296504));
#8340=CARTESIAN_POINT('Ctrl Pts',(-37.4482403780577,32.585837214189,3.33447910373935));
#8341=CARTESIAN_POINT('Ctrl Pts',(-36.4436361477254,29.2581728798308,3.17569438451368));
#8342=CARTESIAN_POINT('Ctrl Pts',(-38.6948242952332,26.6096389957033,3.01690966528799));
#8343=CARTESIAN_POINT('Ctrl Pts',(-42.0751691084,27.0562431709588,2.86115268617591));
#8344=CARTESIAN_POINT('Ctrl Pts',(-43.0738787693705,29.0414198331205,2.75832394680574));
#8345=CARTESIAN_POINT('Ctrl Pts',(-43.0781552224421,30.001056467624,2.70842344717745));
#8346=CARTESIAN_POINT('Ctrl Pts',(-43.0773597741118,29.9982621358397,3.79157655282254));
#8347=CARTESIAN_POINT('Ctrl Pts',(-43.0711552743009,30.9153447223082,3.74392144553925));
#8348=CARTESIAN_POINT('Ctrl Pts',(-42.149452041489,32.8618104304301,3.64333809851406));
#8349=CARTESIAN_POINT('Ctrl Pts',(-38.8394461124454,33.4425494289825,3.48982651174697));
#8350=CARTESIAN_POINT('Ctrl Pts',(-36.4782091884119,30.8916397157027,3.33104179252129));
#8351=CARTESIAN_POINT('Ctrl Pts',(-37.3411135755689,27.5244485680153,3.17225707329561));
#8352=CARTESIAN_POINT('Ctrl Pts',(-40.6381845610556,26.4235838698918,3.01347235406992));
#8353=CARTESIAN_POINT('Ctrl Pts',(-42.8061494447326,28.1603742765857,2.88657884724557));
#8354=CARTESIAN_POINT('Ctrl Pts',(-43.0713227202757,29.590834432844,2.81261358016311));
#8355=CARTESIAN_POINT('Ctrl Pts',(-43.0693700340734,29.9983760594323,2.79157655282254));
#8356=CARTESIAN_POINT('Origin',(-40.,30.,12.2084234471774));
#8357=CARTESIAN_POINT('',(-43.0746299744679,30.0027105195562,4.79157655282254));
#8358=CARTESIAN_POINT('',(-43.0703653163513,29.9977623729938,4.70842344717746));
#8359=CARTESIAN_POINT('',(-43.0735,30.0000000000001,12.2084234471774));
#8360=CARTESIAN_POINT('Ctrl Pts',(-43.0703653163513,29.9977623729938,4.70842344717746));
#8361=CARTESIAN_POINT('Ctrl Pts',(-43.065855939257,30.6666479315962,4.67386791729991));
#8362=CARTESIAN_POINT('Ctrl Pts',(-42.5219682378253,32.3667317756905,4.58638414768047));
#8363=CARTESIAN_POINT('Ctrl Pts',(-39.7160732302253,33.6217974663328,4.44597213831914));
#8364=CARTESIAN_POINT('Ctrl Pts',(-36.802961156292,31.7253909495801,4.28718741909346));
#8365=CARTESIAN_POINT('Ctrl Pts',(-36.8166853311413,28.2494175207298,4.12840269986777));
#8366=CARTESIAN_POINT('Ctrl Pts',(-39.7446814998683,26.3760734330767,3.96961798064209));
#8367=CARTESIAN_POINT('Ctrl Pts',(-42.5322367605161,27.6494461319484,3.82962489641198));
#8368=CARTESIAN_POINT('Ctrl Pts',(-43.0659165451749,29.3412804472297,3.74256005192377));
#8369=CARTESIAN_POINT('Ctrl Pts',(-43.0701873343651,30.0021532462092,3.70842344717745));
#8370=CARTESIAN_POINT('Ctrl Pts',(-43.0746299744679,30.0027105195562,4.79157655282254));
#8371=CARTESIAN_POINT('Ctrl Pts',(-43.0764898067703,30.2050629696594,4.78108579039918));
#8372=CARTESIAN_POINT('Ctrl Pts',(-42.9660571080408,31.4263086365394,4.71766678823391));
#8373=CARTESIAN_POINT('Ctrl Pts',(-41.331906939677,33.379949083163,4.60131954632676));
#8374=CARTESIAN_POINT('Ctrl Pts',(-37.8823642126307,32.9518893225699,4.44253482710107));
#8375=CARTESIAN_POINT('Ctrl Pts',(-36.3714820672996,29.821423650004,4.2837501078754));
#8376=CARTESIAN_POINT('Ctrl Pts',(-38.1824481491975,26.8544416758625,4.1249653886497));
#8377=CARTESIAN_POINT('Ctrl Pts',(-41.6573529260186,26.767166385527,3.96618066942403));
#8378=CARTESIAN_POINT('Ctrl Pts',(-43.0274480390323,28.7774415123474,3.85505105748164));
#8379=CARTESIAN_POINT('Ctrl Pts',(-43.0780463143633,29.8967851225748,3.79684968528114));
#8380=CARTESIAN_POINT('Ctrl Pts',(-43.0773597741118,29.9982621358397,3.79157655282254));
#8381=CARTESIAN_POINT('Origin',(-40.,30.,12.2084234471774));
#8382=CARTESIAN_POINT('',(-43.0685122986719,30.0000666771389,5.79157655282255));
#8383=CARTESIAN_POINT('',(-43.0782644480807,29.9990828882529,5.70842344717746));
#8384=CARTESIAN_POINT('',(-43.0735,30.0000000000001,12.2084234471774));
#8385=CARTESIAN_POINT('Ctrl Pts',(-43.0782644480807,29.9990828882529,5.70842344717746));
#8386=CARTESIAN_POINT('Ctrl Pts',(-43.0744582485572,30.9666843435066,5.65810402241795));
#8387=CARTESIAN_POINT('Ctrl Pts',(-42.060960143324,32.9589222284193,5.55485635791654));
#8388=CARTESIAN_POINT('Ctrl Pts',(-38.6680930907584,33.3799490059277,5.39868045367324));
#8389=CARTESIAN_POINT('Ctrl Pts',(-36.4378892159304,30.7137212758022,5.23989573444757));
#8390=CARTESIAN_POINT('Ctrl Pts',(-37.4687389207455,27.3940935077848,5.08111101522187));
#8391=CARTESIAN_POINT('Ctrl Pts',(-40.81691632925,26.4601300859267,4.92232629599619));
#8392=CARTESIAN_POINT('Ctrl Pts',(-42.8513290865573,28.2648571163145,4.79809710664805));
#8393=CARTESIAN_POINT('Ctrl Pts',(-43.072762891423,29.6421249296032,4.72679615704181));
#8394=CARTESIAN_POINT('Ctrl Pts',(-43.0703653163513,29.9977623729938,4.70842344717746));
#8395=CARTESIAN_POINT('Ctrl Pts',(-43.0685122986719,30.0000666771389,5.79157655282255));
#8396=CARTESIAN_POINT('Ctrl Pts',(-43.0686107637268,30.5090426244347,5.76532189551721));
#8397=CARTESIAN_POINT('Ctrl Pts',(-42.7076773635519,32.0439604140778,5.68613899846998));
#8398=CARTESIAN_POINT('Ctrl Pts',(-40.2839267762627,33.6217975490946,5.55402786168086));
#8399=CARTESIAN_POINT('Ctrl Pts',(-37.1108843622561,32.2025082820388,5.39524314245517));
#8400=CARTESIAN_POINT('Ctrl Pts',(-36.5827795888035,28.7668590664683,5.2364584232295));
#8401=CARTESIAN_POINT('Ctrl Pts',(-39.1830836520825,26.460130005037,5.07767370400381));
#8402=CARTESIAN_POINT('Ctrl Pts',(-42.3100500865757,27.3323873304035,4.9293797472015));
#8403=CARTESIAN_POINT('Ctrl Pts',(-43.0671065373747,29.1841496595299,4.83401403014107));
#8404=CARTESIAN_POINT('Ctrl Pts',(-43.0746299744679,30.0027105195562,4.79157655282254));
#8405=CARTESIAN_POINT('Origin',(-40.,30.,12.2084234471774));
#8406=CARTESIAN_POINT('',(-43.0743851410682,29.9972554299047,6.79157655282255));
#8407=CARTESIAN_POINT('',(-43.0730718382499,30.0028093904244,6.70842344717745));
#8408=CARTESIAN_POINT('',(-43.0735,30.0000000000001,12.2084234471774));
#8409=CARTESIAN_POINT('Ctrl Pts',(-43.0730718382499,30.0028093904244,6.70842344717745));
#8410=CARTESIAN_POINT('Ctrl Pts',(-43.0753733278971,30.2568825879858,6.69526836727787));
#8411=CARTESIAN_POINT('Ctrl Pts',(-42.9303367680532,31.5306038094191,6.6291850476364));
#8412=CARTESIAN_POINT('Ctrl Pts',(-41.1605538610348,33.4425493503161,6.51017348825302));
#8413=CARTESIAN_POINT('Ctrl Pts',(-37.7368491027356,32.8418619451291,6.35138876902735));
#8414=CARTESIAN_POINT('Ctrl Pts',(-36.3850216053963,29.6394968734575,6.19260404980166));
#8415=CARTESIAN_POINT('Ctrl Pts',(-38.3426471118536,26.7671664594007,6.03381933057598));
#8416=CARTESIAN_POINT('Ctrl Pts',(-41.8175518092695,26.8544417477417,5.87503461135029));
#8417=CARTESIAN_POINT('Ctrl Pts',(-43.0546164702181,28.8811768625351,5.76656931688412));
#8418=CARTESIAN_POINT('Ctrl Pts',(-43.0784617808282,29.9489175060867,5.71103226215984));
#8419=CARTESIAN_POINT('Ctrl Pts',(-43.0782644480807,29.9990828882529,5.70842344717746));
#8420=CARTESIAN_POINT('Ctrl Pts',(-43.0743851410682,29.9972554299047,6.79157655282254));
#8421=CARTESIAN_POINT('Ctrl Pts',(-43.0669062988526,30.8079018309698,6.74955800063525));
#8422=CARTESIAN_POINT('Ctrl Pts',(-42.322228951972,32.6518220271502,6.65461120870605));
#8423=CARTESIAN_POINT('Ctrl Pts',(-39.211061602359,33.5462103878864,6.50673617703497));
#8424=CARTESIAN_POINT('Ctrl Pts',(-36.5926235900426,31.2600864669024,6.34795145780927));
#8425=CARTESIAN_POINT('Ctrl Pts',(-37.0935823963814,27.8203742040704,6.1891667385836));
#8426=CARTESIAN_POINT('Ctrl Pts',(-40.2553185059661,26.3760733502665,6.0303820193579));
#8427=CARTESIAN_POINT('Ctrl Pts',(-42.699177866637,27.9396647009882,5.89785195743756));
#8428=CARTESIAN_POINT('Ctrl Pts',(-43.0684122624869,29.4829693968151,5.81825013525911));
#8429=CARTESIAN_POINT('Ctrl Pts',(-43.0685122986719,30.0000666771389,5.79157655282255));
#8430=CARTESIAN_POINT('Origin',(-40.,30.,12.2084234471774));
#8431=CARTESIAN_POINT('',(-43.0775322998549,30.0016204989515,7.79157655282254));
#8432=CARTESIAN_POINT('',(-43.0686900017157,29.9992281658005,7.70842344717746));
#8433=CARTESIAN_POINT('',(-43.0735,30.0000000000001,12.2084234471774));
#8434=CARTESIAN_POINT('Ctrl Pts',(-43.0686900017157,29.9992281658005,7.70842344717746));
#8435=CARTESIAN_POINT('Ctrl Pts',(-43.0674305068904,30.5597738624267,7.67950447239591));
#8436=CARTESIAN_POINT('Ctrl Pts',(-42.6520725496103,32.1479823009103,7.59765725787247));
#8437=CARTESIAN_POINT('Ctrl Pts',(-40.1017542175585,33.6314841495529,7.46288180360712));
#8438=CARTESIAN_POINT('Ctrl Pts',(-37.0039609650845,32.0546974134971,7.30409708438145));
#8439=CARTESIAN_POINT('Ctrl Pts',(-36.6489919521961,28.596869076124,7.14531236515576));
#8440=CARTESIAN_POINT('Ctrl Pts',(-39.3618154535272,26.4235839516209,6.98652764593008));
#8441=CARTESIAN_POINT('Ctrl Pts',(-42.3857288994719,27.4332436093761,6.84089800660397));
#8442=CARTESIAN_POINT('Ctrl Pts',(-43.066113498482,29.2346427220807,6.74819660701977));
#8443=CARTESIAN_POINT('Ctrl Pts',(-43.0730718382499,30.0028093904244,6.70842344717745));
#8444=CARTESIAN_POINT('Ctrl Pts',(-43.0775322998549,30.0016204989515,7.79157655282254));
#8445=CARTESIAN_POINT('Ctrl Pts',(-43.0781297349685,30.0950218669743,7.78672234549517));
#8446=CARTESIAN_POINT('Ctrl Pts',(-43.0319028901288,31.2062331262121,7.72893989842591));
#8447=CARTESIAN_POINT('Ctrl Pts',(-41.6828290582353,33.2196453721168,7.61822921161475));
#8448=CARTESIAN_POINT('Ctrl Pts',(-38.20734371072,33.1598126039199,7.45944449238906));
#8449=CARTESIAN_POINT('Ctrl Pts',(-36.3730052758037,30.2072232146022,7.30065977316339));
#8450=CARTESIAN_POINT('Ctrl Pts',(-37.859120749627,27.0649245856435,7.14187505393769));
#8451=CARTESIAN_POINT('Ctrl Pts',(-41.305175734599,26.6096389182437,6.98309033471202));
#8452=CARTESIAN_POINT('Ctrl Pts',(-42.9606411884153,28.5573021347888,6.86632416767363));
#8453=CARTESIAN_POINT('Ctrl Pts',(-43.0763269459995,29.7867793784346,6.80248624037714));
#8454=CARTESIAN_POINT('Ctrl Pts',(-43.0743851410682,29.9972554299047,6.79157655282254));
#8455=CARTESIAN_POINT('Origin',(-40.,30.,12.2084234471774));
#8456=CARTESIAN_POINT('',(-43.0694985803644,30.001724961275,8.79157655282255));
#8457=CARTESIAN_POINT('',(-43.0759023900792,29.9975851856081,8.70842344717746));
#8458=CARTESIAN_POINT('',(-43.0735,30.0000000000001,12.2084234471774));
#8459=CARTESIAN_POINT('Ctrl Pts',(-43.0759023900792,29.9975851856081,8.70842344717746));
#8460=CARTESIAN_POINT('Ctrl Pts',(-43.0684825656409,30.8585344935406,8.66374057751394));
#8461=CARTESIAN_POINT('Ctrl Pts',(-42.2429728816432,32.751778358711,8.56612946810854));
#8462=CARTESIAN_POINT('Ctrl Pts',(-39.0340360732831,33.502132231285,8.41559011896122));
#8463=CARTESIAN_POINT('Ctrl Pts',(-36.533663382972,31.0874481722331,8.25680539973555));
#8464=CARTESIAN_POINT('Ctrl Pts',(-37.2066643030969,27.6772193954211,8.09802068050986));
#8465=CARTESIAN_POINT('Ctrl Pts',(-40.4369180610355,26.3934598345883,7.93923596128418));
#8466=CARTESIAN_POINT('Ctrl Pts',(-42.7517134474539,28.0439010187842,7.80937021684004));
#8467=CARTESIAN_POINT('Ctrl Pts',(-43.0697356662044,29.5338489379978,7.7324327121378));
#8468=CARTESIAN_POINT('Ctrl Pts',(-43.0686900017157,29.9992281658005,7.70842344717746));
#8469=CARTESIAN_POINT('Ctrl Pts',(-43.0694985803644,30.001724961275,8.79157655282254));
#8470=CARTESIAN_POINT('Ctrl Pts',(-43.0715488058998,30.4011124160455,8.77095845061321));
#8471=CARTESIAN_POINT('Ctrl Pts',(-42.813491762819,31.8232184749255,8.69741210866198));
#8472=CARTESIAN_POINT('Ctrl Pts',(-40.6663948741839,33.5712517973455,8.57093752696885));
#8473=CARTESIAN_POINT('Ctrl Pts',(-37.3607500279849,32.4964767903705,8.41215280774316));
#8474=CARTESIAN_POINT('Ctrl Pts',(-36.4712754607486,29.1361944352982,8.25336808851748));
#8475=CARTESIAN_POINT('Ctrl Pts',(-38.812299668292,26.5667238666358,8.0945833692918));
#8476=CARTESIAN_POINT('Ctrl Pts',(-42.1358312714109,27.1228183719866,7.94065285739349));
#8477=CARTESIAN_POINT('Ctrl Pts',(-43.0716155531895,29.0766125437756,7.83965058523707));
#8478=CARTESIAN_POINT('Ctrl Pts',(-43.0775322998549,30.0016204989515,7.79157655282254));
#8479=CARTESIAN_POINT('Origin',(-40.,30.,12.2084234471774));
#8480=CARTESIAN_POINT('',(-43.070401160077,29.9965365385191,9.79157655282254));
#8481=CARTESIAN_POINT('',(-43.0762854577871,30.0022177574501,9.70842344717746));
#8482=CARTESIAN_POINT('',(-43.0735,30.0000000000001,12.2084234471774));
#8483=CARTESIAN_POINT('',(-40.7937992825329,27.0307770462543,10.));
#8484=CARTESIAN_POINT('Ctrl Pts',(-40.7937992825329,27.0307770462543,10.));
#8485=CARTESIAN_POINT('Ctrl Pts',(-41.7812379463276,27.2947612990625,9.94707176025811));
#8486=CARTESIAN_POINT('Ctrl Pts',(-42.8796301082842,28.3362025511078,9.87759727786562));
#8487=CARTESIAN_POINT('Ctrl Pts',(-43.0728217505486,29.676453251849,9.80812279547313));
#8488=CARTESIAN_POINT('Ctrl Pts',(-43.070401160077,29.9965365385191,9.79157655282254));
#8489=CARTESIAN_POINT('',(-39.2044539122456,27.0254726963224,10.));
#8490=CARTESIAN_POINT('Origin',(-40.,30.,10.));
#8491=CARTESIAN_POINT('Ctrl Pts',(-39.2044525003272,27.0254684088901,10.));
#8492=CARTESIAN_POINT('Ctrl Pts',(-40.1666397594312,26.7696591275303,9.94821753066413));
#8493=CARTESIAN_POINT('Ctrl Pts',(-42.2305611524612,27.2443057138018,9.85102534638995));
#8494=CARTESIAN_POINT('Ctrl Pts',(-43.069053821799,29.1277457869104,9.75383316211576));
#8495=CARTESIAN_POINT('Ctrl Pts',(-43.0762854577871,30.0022177574501,9.70842344717746));
#8496=CARTESIAN_POINT('Origin',(40.,-30.,12.2084234471775));
#8497=CARTESIAN_POINT('',(36.9214106298517,-29.999851864063,0.791576552822544));
#8498=CARTESIAN_POINT('',(36.9314436920733,-29.9992606141577,0.708423447177453));
#8499=CARTESIAN_POINT('',(36.9265,-29.9999999999999,12.2084234471775));
#8500=CARTESIAN_POINT('',(40.7937992825329,-32.9692229537457,0.));
#8501=CARTESIAN_POINT('Ctrl Pts',(36.9314436920733,-29.9992606141577,0.708423447177453));
#8502=CARTESIAN_POINT('Ctrl Pts',(36.9305910605549,-29.5256998684954,0.68399525708588));
#8503=CARTESIAN_POINT('Ctrl Pts',(37.2564685526814,-28.0273013665652,0.606638827252413));
#8504=CARTESIAN_POINT('Ctrl Pts',(39.5908855945796,-26.390973476394,0.47635415767705));
#8505=CARTESIAN_POINT('Ctrl Pts',(42.8129706543341,-27.6976309032298,0.317569438451368));
#8506=CARTESIAN_POINT('Ctrl Pts',(43.4548291366816,-31.1184172884943,0.158784719225683));
#8507=CARTESIAN_POINT('Ctrl Pts',(41.7812379463276,-32.7052387009375,0.0529282397418946));
#8508=CARTESIAN_POINT('Ctrl Pts',(40.7937992825329,-32.9692229537457,0.));
#8509=CARTESIAN_POINT('',(39.2062007174671,-32.9692229537457,0.));
#8510=CARTESIAN_POINT('Origin',(40.,-30.,0.));
#8511=CARTESIAN_POINT('Ctrl Pts',(36.9214106298517,-29.999851864063,0.791576552822544));
#8512=CARTESIAN_POINT('Ctrl Pts',(36.9214062940579,-29.9928656441791,0.791213130185147));
#8513=CARTESIAN_POINT('Ctrl Pts',(36.9245907081615,-28.9684229460631,0.737921467805856));
#8514=CARTESIAN_POINT('Ctrl Pts',(38.0509706569457,-26.9343007433511,0.63170156568467));
#8515=CARTESIAN_POINT('Ctrl Pts',(41.5191018646847,-26.6996618298828,0.472916846458986));
#8516=CARTESIAN_POINT('Ctrl Pts',(43.5964448997665,-29.4874103675251,0.314132127233304));
#8517=CARTESIAN_POINT('Ctrl Pts',(42.3902195200648,-32.7189755800011,0.15649317841364));
#8518=CARTESIAN_POINT('Ctrl Pts',(40.1666405050975,-33.2303412422155,0.0517824693358737));
#8519=CARTESIAN_POINT('Ctrl Pts',(39.2044529144508,-32.9745316477842,-4.47233396150271E-18));
#8520=CARTESIAN_POINT('Origin',(40.,-30.,12.2084234471775));
#8521=CARTESIAN_POINT('',(36.9285656908778,-29.9974006839639,1.79157655282254));
#8522=CARTESIAN_POINT('',(36.9266848795226,-30.0028121938109,1.70842344717745));
#8523=CARTESIAN_POINT('',(36.9265,-29.9999999999999,12.2084234471775));
#8524=CARTESIAN_POINT('Ctrl Pts',(36.9266848795226,-30.0028121938109,1.70842344717745));
#8525=CARTESIAN_POINT('Ctrl Pts',(36.9337738480587,-29.2267098301857,1.66823136220391));
#8526=CARTESIAN_POINT('Ctrl Pts',(37.6258962419323,-27.4173150512511,1.57511103748848));
#8527=CARTESIAN_POINT('Ctrl Pts',(40.6663949504281,-26.4287478255293,1.42906247303115));
#8528=CARTESIAN_POINT('Ctrl Pts',(43.362005411603,-28.6233470492352,1.27027775380547));
#8529=CARTESIAN_POINT('Ctrl Pts',(42.9796778661648,-32.0783451559703,1.11149303457979));
#8530=CARTESIAN_POINT('Ctrl Pts',(39.869659432244,-33.6304611605218,0.952708315354101));
#8531=CARTESIAN_POINT('Ctrl Pts',(37.3388061489086,-32.1318111502224,0.818351786219991));
#8532=CARTESIAN_POINT('Ctrl Pts',(36.932438446106,-30.5517577378998,0.736923496827775));
#8533=CARTESIAN_POINT('Ctrl Pts',(36.9314436920733,-29.9992606141577,0.708423447177453));
#8534=CARTESIAN_POINT('Ctrl Pts',(36.9285656908778,-29.9974006839639,1.79157655282254));
#8535=CARTESIAN_POINT('Ctrl Pts',(36.9260625923045,-29.6855009021205,1.77544923530318));
#8536=CARTESIAN_POINT('Ctrl Pts',(37.1131654440729,-28.3529099953329,1.70639367804192));
#8537=CARTESIAN_POINT('Ctrl Pts',(39.034036182301,-26.4978681661549,1.58440988103877));
#8538=CARTESIAN_POINT('Ctrl Pts',(42.4187331109537,-27.2893204582939,1.42562516181309));
#8539=CARTESIAN_POINT('Ctrl Pts',(43.5891186388302,-30.5623706046428,1.26684044258741));
#8540=CARTESIAN_POINT('Ctrl Pts',(41.4737277243454,-33.3205487833603,1.10805572336172));
#8541=CARTESIAN_POINT('Ctrl Pts',(38.0170882892501,-33.039525905726,0.949634426773433));
#8542=CARTESIAN_POINT('Ctrl Pts',(36.9220377515051,-31.0103265364098,0.844141369927042));
#8543=CARTESIAN_POINT('Ctrl Pts',(36.9214106298517,-29.999851864063,0.791576552822544));
#8544=CARTESIAN_POINT('Origin',(40.,-30.,12.2084234471775));
#8545=CARTESIAN_POINT('',(36.9306303788003,-30.0016239403382,2.79157655282254));
#8546=CARTESIAN_POINT('',(36.9218444103647,-29.9989435321732,2.70842344717745));
#8547=CARTESIAN_POINT('',(36.9265,-29.9999999999999,12.2084234471775));
#8548=CARTESIAN_POINT('Ctrl Pts',(36.9218444103647,-29.9989435321732,2.70842344717745));
#8549=CARTESIAN_POINT('Ctrl Pts',(36.921584934203,-29.9407170474496,2.70539570706384));
#8550=CARTESIAN_POINT('Ctrl Pts',(36.9494735790417,-28.8648808025215,2.64943972720834));
#8551=CARTESIAN_POINT('Ctrl Pts',(38.2073435376042,-26.840187091708,2.54055550761094));
#8552=CARTESIAN_POINT('Ctrl Pts',(41.682829220934,-26.7803543165819,2.38177078838526));
#8553=CARTESIAN_POINT('Ctrl Pts',(43.61771316324,-29.668053222969,2.22298606915957));
#8554=CARTESIAN_POINT('Ctrl Pts',(42.2406392443386,-32.8596454297127,2.06420134993389));
#8555=CARTESIAN_POINT('Ctrl Pts',(38.8122995514484,-33.4332764695832,1.9054166307082));
#8556=CARTESIAN_POINT('Ctrl Pts',(37.063842552554,-31.5141981352583,1.78682399645606));
#8557=CARTESIAN_POINT('Ctrl Pts',(36.9244385118489,-30.248745188472,1.72115960194581));
#8558=CARTESIAN_POINT('Ctrl Pts',(36.9266848795226,-30.0028121938109,1.70842344717745));
#8559=CARTESIAN_POINT('Ctrl Pts',(36.9306303788003,-30.0016239403382,2.79157655282254));
#8560=CARTESIAN_POINT('Ctrl Pts',(36.9335905651907,-29.3838087605833,2.75968534042121));
#8561=CARTESIAN_POINT('Ctrl Pts',(37.4143808562999,-27.7363979405694,2.67486588827799));
#8562=CARTESIAN_POINT('Ctrl Pts',(40.1017542062109,-26.3685162560978,2.53711819639287));
#8563=CARTESIAN_POINT('Ctrl Pts',(43.1063928273453,-28.1162929520197,2.37833347716719));
#8564=CARTESIAN_POINT('Ctrl Pts',(43.2671801112825,-31.58857257803,2.2195487579415));
#8565=CARTESIAN_POINT('Ctrl Pts',(40.4369180121167,-33.6065397617092,2.06076403871582));
#8566=CARTESIAN_POINT('Ctrl Pts',(37.5347523711613,-32.4531681815965,1.9181066370095));
#8567=CARTESIAN_POINT('Ctrl Pts',(36.9342775109495,-30.7091247260472,1.82837747504507));
#8568=CARTESIAN_POINT('Ctrl Pts',(36.9285656908778,-29.9974006839639,1.79157655282254));
#8569=CARTESIAN_POINT('Origin',(40.,-30.,12.2084234471775));
#8570=CARTESIAN_POINT('',(36.9226406398379,-30.0017378639268,3.79157655282254));
#8571=CARTESIAN_POINT('',(36.9298122993513,-29.9978467535325,3.70842344717745));
#8572=CARTESIAN_POINT('',(36.9265,-29.9999999999999,12.2084234471775));
#8573=CARTESIAN_POINT('Ctrl Pts',(36.9298122993513,-29.9978467535325,3.70842344717745));
#8574=CARTESIAN_POINT('Ctrl Pts',(36.9274613004229,-29.634047190253,3.68963181218188));
#8575=CARTESIAN_POINT('Ctrl Pts',(37.155552695261,-28.2484270985199,3.61791193744441));
#8576=CARTESIAN_POINT('Ctrl Pts',(39.211061526259,-26.4537892700808,3.49326382296504));
#8577=CARTESIAN_POINT('Ctrl Pts',(42.5517599263879,-27.4141624772917,3.33447910373936));
#8578=CARTESIAN_POINT('Ctrl Pts',(43.5563642765403,-30.7418272087093,3.17569438451367));
#8579=CARTESIAN_POINT('Ctrl Pts',(41.3051758605191,-33.3903614087074,3.01690966528799));
#8580=CARTESIAN_POINT('Ctrl Pts',(37.9248306439518,-32.9437571803748,2.86115268617591));
#8581=CARTESIAN_POINT('Ctrl Pts',(36.9261208639649,-30.9585802811283,2.75832394680574));
#8582=CARTESIAN_POINT('Ctrl Pts',(36.9218444103647,-29.9989435321732,2.70842344717745));
#8583=CARTESIAN_POINT('Ctrl Pts',(36.9226406398379,-30.0017378639268,3.79157655282254));
#8584=CARTESIAN_POINT('Ctrl Pts',(36.9288451388142,-29.0846554008188,3.74392144553925));
#8585=CARTESIAN_POINT('Ctrl Pts',(37.8505482476435,-27.1381899545233,3.64333809851406));
#8586=CARTESIAN_POINT('Ctrl Pts',(41.1605537314434,-26.5574510340941,3.48982651174697));
#8587=CARTESIAN_POINT('Ctrl Pts',(43.5217903378555,-29.1083604042289,3.33104179252129));
#8588=CARTESIAN_POINT('Ctrl Pts',(42.6588860667731,-32.4755510990005,3.17225707329561));
#8589=CARTESIAN_POINT('Ctrl Pts',(39.3618155247875,-33.5764156490026,3.01347235406992));
#8590=CARTESIAN_POINT('Ctrl Pts',(37.1938509327382,-31.8396254759918,2.88657884724557));
#8591=CARTESIAN_POINT('Ctrl Pts',(36.9286776928615,-30.4091655121155,2.81261358016311));
#8592=CARTESIAN_POINT('Ctrl Pts',(36.9306303788003,-30.0016239403382,2.79157655282254));
#8593=CARTESIAN_POINT('Origin',(40.,-30.,12.2084234471775));
#8594=CARTESIAN_POINT('',(36.9253704391146,-29.9972894808084,4.79157655282255));
#8595=CARTESIAN_POINT('',(36.929634317343,-30.0022376272732,4.70842344717745));
#8596=CARTESIAN_POINT('',(36.9265,-29.9999999999999,12.2084234471775));
#8597=CARTESIAN_POINT('Ctrl Pts',(36.929634317343,-30.0022376272731,4.70842344717745));
#8598=CARTESIAN_POINT('Ctrl Pts',(36.9341436949753,-29.3333519888702,4.67386791729991));
#8599=CARTESIAN_POINT('Ctrl Pts',(37.4780314612948,-27.6332679419497,4.58638414768048));
#8600=CARTESIAN_POINT('Ctrl Pts',(40.2839268036481,-26.3782021015739,4.44597213831914));
#8601=CARTESIAN_POINT('Ctrl Pts',(43.1970392251266,-28.2746088445741,4.28718741909346));
#8602=CARTESIAN_POINT('Ctrl Pts',(43.1833150486392,-31.7505826881217,4.12840269986777));
#8603=CARTESIAN_POINT('Ctrl Pts',(40.2553185305929,-33.6239269992694,3.9696179806421));
#8604=CARTESIAN_POINT('Ctrl Pts',(37.4677629373775,-32.3505541484834,3.82962489641198));
#8605=CARTESIAN_POINT('Ctrl Pts',(36.9340830890508,-30.6587196313569,3.74256005192377));
#8606=CARTESIAN_POINT('Ctrl Pts',(36.9298122993513,-29.9978467535325,3.70842344717745));
#8607=CARTESIAN_POINT('Ctrl Pts',(36.9253704391146,-29.9972894808084,4.79157655282255));
#8608=CARTESIAN_POINT('Ctrl Pts',(36.9235106070623,-29.7949370579245,4.78108579039918));
#8609=CARTESIAN_POINT('Ctrl Pts',(37.0339432909371,-28.5736915553199,4.71766678823392));
#8610=CARTESIAN_POINT('Ctrl Pts',(38.6680932394838,-26.6200513714892,4.60131954632676));
#8611=CARTESIAN_POINT('Ctrl Pts',(42.1176355025165,-27.0481110745022,4.44253482710108));
#8612=CARTESIAN_POINT('Ctrl Pts',(43.6285174446119,-30.1785763259747,4.28375010787539));
#8613=CARTESIAN_POINT('Ctrl Pts',(41.8175516063153,-33.1455579010144,4.12496538864971));
#8614=CARTESIAN_POINT('Ctrl Pts',(38.3426472969195,-33.2328331796093,3.96618066942402));
#8615=CARTESIAN_POINT('Ctrl Pts',(36.9725523682035,-31.2225583232012,3.85505105748164));
#8616=CARTESIAN_POINT('Ctrl Pts',(36.9219540996787,-30.1032148635415,3.79684968528114));
#8617=CARTESIAN_POINT('Ctrl Pts',(36.9226406398379,-30.0017378639268,3.79157655282254));
#8618=CARTESIAN_POINT('Origin',(40.,-30.,12.2084234471775));
#8619=CARTESIAN_POINT('',(36.9314881140875,-29.9999333228699,5.79157655282255));
#8620=CARTESIAN_POINT('',(36.9217351846713,-30.0009171118566,5.70842344717746));
#8621=CARTESIAN_POINT('',(36.9265,-29.9999999999999,12.2084234471775));
#8622=CARTESIAN_POINT('Ctrl Pts',(36.9217351846712,-30.0009171118566,5.70842344717746));
#8623=CARTESIAN_POINT('Ctrl Pts',(36.9255413846488,-29.0333155411646,5.65810402241795));
#8624=CARTESIAN_POINT('Ctrl Pts',(37.939039610796,-27.0410774185704,5.55485635791655));
#8625=CARTESIAN_POINT('Ctrl Pts',(41.3319070681429,-26.6200505908322,5.39868045367324));
#8626=CARTESIAN_POINT('Ctrl Pts',(43.5621112090423,-29.2862786390484,5.23989573444757));
#8627=CARTESIAN_POINT('Ctrl Pts',(42.531261381243,-32.6059068031093,5.08111101522187));
#8628=CARTESIAN_POINT('Ctrl Pts',(39.1830835732889,-33.5398703363926,4.92232629599619));
#8629=CARTESIAN_POINT('Ctrl Pts',(37.1486705732688,-31.7351430906943,4.79809710664805));
#8630=CARTESIAN_POINT('Ctrl Pts',(36.9272367419853,-30.3578751130926,4.7267961570418));
#8631=CARTESIAN_POINT('Ctrl Pts',(36.929634317343,-30.0022376272731,4.70842344717745));
#8632=CARTESIAN_POINT('Ctrl Pts',(36.9314881140875,-29.9999333228699,5.79157655282255));
#8633=CARTESIAN_POINT('Ctrl Pts',(36.931389649046,-29.4909574440388,5.76532189551721));
#8634=CARTESIAN_POINT('Ctrl Pts',(37.2923230006704,-27.956039860865,5.68613899846999));
#8635=CARTESIAN_POINT('Ctrl Pts',(39.7160732619294,-26.3782029380897,5.55402786168086));
#8636=CARTESIAN_POINT('Ctrl Pts',(42.8891152491159,-27.7974920142308,5.39524314245518));
#8637=CARTESIAN_POINT('Ctrl Pts',(43.4172199515306,-31.2331407676563,5.2364584232295));
#8638=CARTESIAN_POINT('Ctrl Pts',(40.8169162380303,-33.5398695187991,5.07767370400381));
#8639=CARTESIAN_POINT('Ctrl Pts',(37.6899502241597,-32.6676123107638,4.92937974720149));
#8640=CARTESIAN_POINT('Ctrl Pts',(36.9328938751957,-30.8158502307263,4.83401403014107));
#8641=CARTESIAN_POINT('Ctrl Pts',(36.9253704391146,-29.9972894808084,4.79157655282255));
#8642=CARTESIAN_POINT('Origin',(40.,-30.,12.2084234471775));
#8643=CARTESIAN_POINT('',(36.9256152724736,-30.0027445697125,6.79157655282255));
#8644=CARTESIAN_POINT('',(36.9269277951216,-29.9971906092403,6.70842344717746));
#8645=CARTESIAN_POINT('',(36.9265,-29.9999999999999,12.2084234471775));
#8646=CARTESIAN_POINT('Ctrl Pts',(36.9269277951216,-29.9971906092403,6.70842344717746));
#8647=CARTESIAN_POINT('Ctrl Pts',(36.9246263051997,-29.7431173813678,6.69526836727788));
#8648=CARTESIAN_POINT('Ctrl Pts',(37.0696628823468,-28.4693960079781,6.6291850476364));
#8649=CARTESIAN_POINT('Ctrl Pts',(38.8394460005071,-26.5574502389721,6.51017348825302));
#8650=CARTESIAN_POINT('Ctrl Pts',(42.2631511672664,-27.1581377158282,6.35138876902735));
#8651=CARTESIAN_POINT('Ctrl Pts',(43.6149788258837,-30.3605031695509,6.19260404980166));
#8652=CARTESIAN_POINT('Ctrl Pts',(41.6573530858745,-33.2328339262885,6.03381933057598));
#8653=CARTESIAN_POINT('Ctrl Pts',(38.1824479738899,-33.1455586275345,5.87503461135029));
#8654=CARTESIAN_POINT('Ctrl Pts',(36.9453831653551,-31.1188232709446,5.76656931688412));
#8655=CARTESIAN_POINT('Ctrl Pts',(36.9215378519002,-30.0510825000077,5.71103226215984));
#8656=CARTESIAN_POINT('Ctrl Pts',(36.9217351846712,-30.0009171118566,5.70842344717746));
#8657=CARTESIAN_POINT('Ctrl Pts',(36.9256152724736,-30.0027445697125,6.79157655282255));
#8658=CARTESIAN_POINT('Ctrl Pts',(36.9330941136838,-29.192098277692,6.74955800063525));
#8659=CARTESIAN_POINT('Ctrl Pts',(37.6777713604131,-27.3481783295783,6.65461120870605));
#8660=CARTESIAN_POINT('Ctrl Pts',(40.7889382915105,-26.453790089119,6.50673617703496));
#8661=CARTESIAN_POINT('Ctrl Pts',(43.4073759516192,-28.7399137026036,6.34795145780928));
#8662=CARTESIAN_POINT('Ctrl Pts',(42.9064172126614,-32.1796255027351,6.18916673858359));
#8663=CARTESIAN_POINT('Ctrl Pts',(39.7446815283789,-33.6239261622643,6.03038201935791));
#8664=CARTESIAN_POINT('Ctrl Pts',(37.3008224964414,-32.0603350218663,5.89785195743756));
#8665=CARTESIAN_POINT('Ctrl Pts',(36.9315881502591,-30.5170305336365,5.81825013525911));
#8666=CARTESIAN_POINT('Ctrl Pts',(36.9314881140875,-29.9999333228699,5.79157655282255));
#8667=CARTESIAN_POINT('Origin',(40.,-30.,12.2084234471775));
#8668=CARTESIAN_POINT('',(36.9224681139214,-29.9983795008932,7.79157655282255));
#8669=CARTESIAN_POINT('',(36.9313096321944,-30.0007718341681,7.70842344717745));
#8670=CARTESIAN_POINT('',(36.9265,-29.9999999999999,12.2084234471775));
#8671=CARTESIAN_POINT('Ctrl Pts',(36.9313096321944,-30.0007718341681,7.70842344717745));
#8672=CARTESIAN_POINT('Ctrl Pts',(36.932569127163,-29.4402260707305,7.67950447239591));
#8673=CARTESIAN_POINT('Ctrl Pts',(37.3479271339629,-27.8520174430537,7.59765725787246));
#8674=CARTESIAN_POINT('Ctrl Pts',(39.8982457703173,-26.3685154170426,7.46288180360713));
#8675=CARTESIAN_POINT('Ctrl Pts',(42.9960393923464,-27.9453023414519,7.30409708438144));
#8676=CARTESIAN_POINT('Ctrl Pts',(43.3510084475949,-31.4031310912316,7.14531236515576));
#8677=CARTESIAN_POINT('Ctrl Pts',(40.6381846226088,-33.576416475081,6.98652764593008));
#8678=CARTESIAN_POINT('Ctrl Pts',(37.6142708159026,-32.5667566968382,6.84089800660397));
#8679=CARTESIAN_POINT('Ctrl Pts',(36.9338861357197,-30.7653573692269,6.74819660701977));
#8680=CARTESIAN_POINT('Ctrl Pts',(36.9269277951216,-29.9971906092403,6.70842344717746));
#8681=CARTESIAN_POINT('Ctrl Pts',(36.9224681139214,-29.9983795008932,7.79157655282255));
#8682=CARTESIAN_POINT('Ctrl Pts',(36.9218706788586,-29.9049781453709,7.78672234549517));
#8683=CARTESIAN_POINT('Ctrl Pts',(36.9680975171812,-28.7937670349628,7.7289398984259));
#8684=CARTESIAN_POINT('Ctrl Pts',(38.3171711686706,-26.7803550620374,7.61822921161474));
#8685=CARTESIAN_POINT('Ctrl Pts',(41.7926560478477,-26.8401878205589,7.45944449238907));
#8686=CARTESIAN_POINT('Ctrl Pts',(43.6269942364715,-29.7927768135681,7.30065977316338));
#8687=CARTESIAN_POINT('Ctrl Pts',(42.1408789623084,-32.935075019391,7.1418750539377));
#8688=CARTESIAN_POINT('Ctrl Pts',(38.6948244410116,-33.3903606257847,6.98309033471201));
#8689=CARTESIAN_POINT('Ctrl Pts',(37.0393592098282,-31.4426976711376,6.86632416767363));
#8690=CARTESIAN_POINT('Ctrl Pts',(36.9236734678033,-30.2132205928703,6.80248624037714));
#8691=CARTESIAN_POINT('Ctrl Pts',(36.9256152724736,-30.0027445697125,6.79157655282255));
#8692=CARTESIAN_POINT('Origin',(40.,-30.,12.2084234471775));
#8693=CARTESIAN_POINT('',(36.9305018352452,-29.9982750548043,8.79157655282255));
#8694=CARTESIAN_POINT('',(36.9240972445879,-30.002414807271,8.70842344717745));
#8695=CARTESIAN_POINT('',(36.9265,-29.9999999999999,12.2084234471775));
#8696=CARTESIAN_POINT('Ctrl Pts',(36.9240972445879,-30.002414807271,8.70842344717746));
#8697=CARTESIAN_POINT('Ctrl Pts',(36.9315170701463,-29.1414653963739,8.66374057751394));
#8698=CARTESIAN_POINT('Ctrl Pts',(37.7570268484348,-27.248221324497,8.56612946810854));
#8699=CARTESIAN_POINT('Ctrl Pts',(40.9659640431824,-26.4978673441227,8.41559011896122));
#8700=CARTESIAN_POINT('Ctrl Pts',(43.4663370299824,-28.9125517016798,8.25680539973555));
#8701=CARTESIAN_POINT('Ctrl Pts',(42.7933360304446,-32.322780879739,8.09802068050986));
#8702=CARTESIAN_POINT('Ctrl Pts',(39.5630818867002,-33.6065405967288,7.93923596128418));
#8703=CARTESIAN_POINT('Ctrl Pts',(37.2482862242861,-31.9560992143217,7.80937021684005));
#8704=CARTESIAN_POINT('Ctrl Pts',(36.9302639675868,-30.4661511174393,7.7324327121378));
#8705=CARTESIAN_POINT('Ctrl Pts',(36.9313096321944,-30.0007718341681,7.70842344717745));
#8706=CARTESIAN_POINT('Ctrl Pts',(36.9305018352452,-29.9982750548043,8.79157655282255));
#8707=CARTESIAN_POINT('Ctrl Pts',(36.9284516052967,-29.598887638351,8.77095845061321));
#8708=CARTESIAN_POINT('Ctrl Pts',(37.186508597033,-28.1767817125267,8.69741210866198));
#8709=CARTESIAN_POINT('Ctrl Pts',(39.3336052322159,-26.4287487288557,8.57093752696886));
#8710=CARTESIAN_POINT('Ctrl Pts',(42.6392496071423,-27.5035235206868,8.41215280774315));
#8711=CARTESIAN_POINT('Ctrl Pts',(43.5287240702543,-30.8638054618116,8.25336808851749));
#8712=CARTESIAN_POINT('Ctrl Pts',(41.1877001687398,-33.4332756644217,8.09458336929179));
#8713=CARTESIAN_POINT('Ctrl Pts',(37.8641690175257,-32.8771812444488,7.94065285739349));
#8714=CARTESIAN_POINT('Ctrl Pts',(36.9283848600841,-30.9233873322688,7.83965058523707));
#8715=CARTESIAN_POINT('Ctrl Pts',(36.9224681139214,-29.9983795008932,7.79157655282255));
#8716=CARTESIAN_POINT('Origin',(40.,-30.,12.2084234471775));
#8717=CARTESIAN_POINT('',(36.9295986129496,-30.0034658759783,9.79157655282255));
#8718=CARTESIAN_POINT('',(36.9237142109313,-29.9977821171135,9.70842344717746));
#8719=CARTESIAN_POINT('',(36.9265,-29.9999999999999,12.2084234471775));
#8720=CARTESIAN_POINT('',(39.2062007174671,-32.9692229537457,10.));
#8721=CARTESIAN_POINT('Ctrl Pts',(39.2062007174671,-32.9692229537457,10.));
#8722=CARTESIAN_POINT('Ctrl Pts',(38.2187620536724,-32.7052387009375,9.94707176025811));
#8723=CARTESIAN_POINT('Ctrl Pts',(37.1203692887103,-31.663801299125,9.87759727786562));
#8724=CARTESIAN_POINT('Ctrl Pts',(36.9271779329065,-30.3235495409403,9.80812279547314));
#8725=CARTESIAN_POINT('Ctrl Pts',(36.9295986129496,-30.0034658759783,9.79157655282254));
#8726=CARTESIAN_POINT('',(40.7955465233069,-32.9745272340617,10.));
#8727=CARTESIAN_POINT('Origin',(40.,-30.,10.));
#8728=CARTESIAN_POINT('Ctrl Pts',(40.795547939453,-32.9745315332036,10.));
#8729=CARTESIAN_POINT('Ctrl Pts',(39.8333610342226,-33.2303404802746,9.94821753066413));
#8730=CARTESIAN_POINT('Ctrl Pts',(37.7694379004992,-32.755695571864,9.85102534638994));
#8731=CARTESIAN_POINT('Ctrl Pts',(36.9309457034163,-30.8722543866673,9.75383316211577));
#8732=CARTESIAN_POINT('Ctrl Pts',(36.9237142109313,-29.9977821171135,9.70842344717746));
#8733=CARTESIAN_POINT('Origin',(-40.,-30.,12.2084234471775));
#8734=CARTESIAN_POINT('',(-43.0785899477782,-29.9998519260269,0.791576552822544));
#8735=CARTESIAN_POINT('',(-43.0685561331992,-29.9992605379075,0.708423447177453));
#8736=CARTESIAN_POINT('',(-43.0735,-29.9999999999999,12.2084234471775));
#8737=CARTESIAN_POINT('',(-39.2062007174671,-32.9692229537457,0.));
#8738=CARTESIAN_POINT('Ctrl Pts',(-43.0685561331992,-29.9992605379075,0.708423447177453));
#8739=CARTESIAN_POINT('Ctrl Pts',(-43.0694087586157,-29.525699780414,0.683995257085881));
#8740=CARTESIAN_POINT('Ctrl Pts',(-42.7435312639193,-28.0273012908912,0.606638827252414));
#8741=CARTESIAN_POINT('Ctrl Pts',(-40.4091143639642,-26.3909743325875,0.47635415767705));
#8742=CARTESIAN_POINT('Ctrl Pts',(-37.1870296834247,-27.6976298827388,0.317569438451369));
#8743=CARTESIAN_POINT('Ctrl Pts',(-36.5451704756118,-31.1184197653857,0.158784719225683));
#8744=CARTESIAN_POINT('Ctrl Pts',(-38.2187620536724,-32.7052387009375,0.0529282397418946));
#8745=CARTESIAN_POINT('Ctrl Pts',(-39.2062007174671,-32.9692229537457,0.));
#8746=CARTESIAN_POINT('',(-40.7937992825329,-32.9692229537457,0.));
#8747=CARTESIAN_POINT('Origin',(-40.,-30.,0.));
#8748=CARTESIAN_POINT('Ctrl Pts',(-43.0785899477782,-29.9998519260269,0.791576552822544));
#8749=CARTESIAN_POINT('Ctrl Pts',(-43.0785942836995,-29.9928657045085,0.791213130185147));
#8750=CARTESIAN_POINT('Ctrl Pts',(-43.0754098879479,-28.9684227656317,0.737921467805856));
#8751=CARTESIAN_POINT('Ctrl Pts',(-41.9490298715236,-26.9342997681684,0.631701565684669));
#8752=CARTESIAN_POINT('Ctrl Pts',(-38.4808975311013,-26.6996618476225,0.472916846458986));
#8753=CARTESIAN_POINT('Ctrl Pts',(-36.4035550403569,-29.4874091667537,0.314132127233303));
#8754=CARTESIAN_POINT('Ctrl Pts',(-37.6097787213515,-32.7189778808771,0.156493178413639));
#8755=CARTESIAN_POINT('Ctrl Pts',(-39.8333607858277,-33.2303406028725,0.051782469335873));
#8756=CARTESIAN_POINT('Ctrl Pts',(-40.7955478019228,-32.974531551058,4.67562186884374E-17));
#8757=CARTESIAN_POINT('Origin',(-40.,-30.,12.2084234471775));
#8758=CARTESIAN_POINT('',(-43.071434903389,-29.9974006852265,1.79157655282254));
#8759=CARTESIAN_POINT('',(-43.0733149456894,-30.0028121937047,1.70842344717745));
#8760=CARTESIAN_POINT('',(-43.0735,-29.9999999999999,12.2084234471775));
#8761=CARTESIAN_POINT('Ctrl Pts',(-43.0733149456894,-30.0028121937047,1.70842344717745));
#8762=CARTESIAN_POINT('Ctrl Pts',(-43.0662259767823,-29.2267098723251,1.66823136220391));
#8763=CARTESIAN_POINT('Ctrl Pts',(-42.3741036197155,-27.4173151902012,1.57511103748848));
#8764=CARTESIAN_POINT('Ctrl Pts',(-39.333605094551,-26.4287480480142,1.42906247303115));
#8765=CARTESIAN_POINT('Ctrl Pts',(-36.6379947680772,-28.6233470921482,1.27027775380547));
#8766=CARTESIAN_POINT('Ctrl Pts',(-37.0203223217504,-32.078345102403,1.11149303457979));
#8767=CARTESIAN_POINT('Ctrl Pts',(-40.1303405334711,-33.6304608367794,0.952708315354102));
#8768=CARTESIAN_POINT('Ctrl Pts',(-42.661193724397,-32.1318111884618,0.81835178621999));
#8769=CARTESIAN_POINT('Ctrl Pts',(-43.0675613862855,-30.5517576754528,0.736923496827775));
#8770=CARTESIAN_POINT('Ctrl Pts',(-43.0685561331992,-29.9992605379075,0.708423447177453));
#8771=CARTESIAN_POINT('Ctrl Pts',(-43.071434903389,-29.9974006852265,1.79157655282254));
#8772=CARTESIAN_POINT('Ctrl Pts',(-43.0739380024191,-29.6855008432268,1.77544923530318));
#8773=CARTESIAN_POINT('Ctrl Pts',(-42.8868351144726,-28.3529096785031,1.70639367804192));
#8774=CARTESIAN_POINT('Ctrl Pts',(-40.9659640066834,-26.4978674771854,1.58440988103877));
#8775=CARTESIAN_POINT('Ctrl Pts',(-37.5812664167199,-27.2893199539358,1.42562516181309));
#8776=CARTESIAN_POINT('Ctrl Pts',(-36.410880674872,-30.5623706761659,1.26684044258741));
#8777=CARTESIAN_POINT('Ctrl Pts',(-38.5262719729362,-33.320549494049,1.10805572336172));
#8778=CARTESIAN_POINT('Ctrl Pts',(-41.9829121303265,-33.0395263722366,0.949634426773433));
#8779=CARTESIAN_POINT('Ctrl Pts',(-43.0779628076698,-31.0103268347954,0.844141369927042));
#8780=CARTESIAN_POINT('Ctrl Pts',(-43.0785899477782,-29.9998519260269,0.791576552822544));
#8781=CARTESIAN_POINT('Origin',(-40.,-30.,12.2084234471775));
#8782=CARTESIAN_POINT('',(-43.0693702153585,-30.0016239406685,2.79157655282254));
#8783=CARTESIAN_POINT('',(-43.078155414487,-29.9989435322699,2.70842344717745));
#8784=CARTESIAN_POINT('',(-43.0735,-29.9999999999999,12.2084234471775));
#8785=CARTESIAN_POINT('Ctrl Pts',(-43.078155414487,-29.9989435322699,2.70842344717745));
#8786=CARTESIAN_POINT('Ctrl Pts',(-43.0784148906334,-29.9407170508587,2.70539570706384));
#8787=CARTESIAN_POINT('Ctrl Pts',(-43.0505262473693,-28.8648808671286,2.64943972720834));
#8788=CARTESIAN_POINT('Ctrl Pts',(-41.7926563602578,-26.8401872712874,2.54055550761094));
#8789=CARTESIAN_POINT('Ctrl Pts',(-38.3171708750578,-26.7803545002487,2.38177078838525));
#8790=CARTESIAN_POINT('Ctrl Pts',(-36.3822870422175,-29.6680532410143,2.22298606915957));
#8791=CARTESIAN_POINT('Ctrl Pts',(-37.7593608839214,-32.8596452685709,2.06420134993389));
#8792=CARTESIAN_POINT('Ctrl Pts',(-41.1877003796151,-33.4332762712177,1.9054166307082));
#8793=CARTESIAN_POINT('Ctrl Pts',(-42.9361572817983,-31.5141980525073,1.78682399645606));
#8794=CARTESIAN_POINT('Ctrl Pts',(-43.0755613134807,-30.248745174979,1.72115960194581));
#8795=CARTESIAN_POINT('Ctrl Pts',(-43.0733149456894,-30.0028121937047,1.70842344717745));
#8796=CARTESIAN_POINT('Ctrl Pts',(-43.0693702153585,-30.0016239406685,2.79157655282254));
#8797=CARTESIAN_POINT('Ctrl Pts',(-43.0664100283933,-29.3838086413388,2.75968534042121));
#8798=CARTESIAN_POINT('Ctrl Pts',(-42.5856196442103,-27.7363975024695,2.67486588827799));
#8799=CARTESIAN_POINT('Ctrl Pts',(-39.898245774117,-26.3685155528715,2.53711819639287));
#8800=CARTESIAN_POINT('Ctrl Pts',(-36.8936065712748,-28.1162925878559,2.37833347716719));
#8801=CARTESIAN_POINT('Ctrl Pts',(-36.7328192563745,-31.5885728846373,2.2195487579415));
#8802=CARTESIAN_POINT('Ctrl Pts',(-39.5630819030797,-33.6065404615547,2.06076403871582));
#8803=CARTESIAN_POINT('Ctrl Pts',(-42.4652481064523,-32.4531686537838,1.9181066370095));
#8804=CARTESIAN_POINT('Ctrl Pts',(-43.0657230822749,-30.7091248645808,1.82837747504507));
#8805=CARTESIAN_POINT('Ctrl Pts',(-43.071434903389,-29.9974006852265,1.79157655282254));
#8806=CARTESIAN_POINT('Origin',(-40.,-30.,12.2084234471775));
#8807=CARTESIAN_POINT('',(-43.0773599558693,-30.0017378642629,3.79157655282254));
#8808=CARTESIAN_POINT('',(-43.0701875259343,-29.9978467536557,3.70842344717745));
#8809=CARTESIAN_POINT('',(-43.0735,-29.9999999999999,12.2084234471775));
#8810=CARTESIAN_POINT('Ctrl Pts',(-43.0701875259343,-29.9978467536557,3.70842344717745));
#8811=CARTESIAN_POINT('Ctrl Pts',(-43.0725385247289,-29.6340472110791,3.68963181218188));
#8812=CARTESIAN_POINT('Ctrl Pts',(-42.8444471428709,-28.2484271981974,3.61791193744441));
#8813=CARTESIAN_POINT('Ctrl Pts',(-40.7889384288422,-26.4537894718797,3.49326382296504));
#8814=CARTESIAN_POINT('Ctrl Pts',(-37.4482402188302,-27.414162624453,3.33447910373936));
#8815=CARTESIAN_POINT('Ctrl Pts',(-36.4436359258312,-30.7418271664764,3.17569438451367));
#8816=CARTESIAN_POINT('Ctrl Pts',(-38.6948242137735,-33.3903612158066,3.01690966528799));
#8817=CARTESIAN_POINT('Ctrl Pts',(-42.0751692379219,-32.9437570127916,2.86115268617591));
#8818=CARTESIAN_POINT('Ctrl Pts',(-43.0738789611389,-30.9585802266324,2.75832394680574));
#8819=CARTESIAN_POINT('Ctrl Pts',(-43.078155414487,-29.9989435322699,2.70842344717745));
#8820=CARTESIAN_POINT('Ctrl Pts',(-43.0773599558693,-30.0017378642629,3.79157655282254));
#8821=CARTESIAN_POINT('Ctrl Pts',(-43.0711554556919,-29.084655223629,3.74392144553925));
#8822=CARTESIAN_POINT('Ctrl Pts',(-42.1494521684416,-27.1381894005441,3.64333809851406));
#8823=CARTESIAN_POINT('Ctrl Pts',(-38.8394460438999,-26.5574503676893,3.48982651174697));
#8824=CARTESIAN_POINT('Ctrl Pts',(-36.4782089804049,-29.1083602316377,3.33104179252129));
#8825=CARTESIAN_POINT('Ctrl Pts',(-37.341113418528,-32.4755515781919,3.17225707329561));
#8826=CARTESIAN_POINT('Ctrl Pts',(-40.6381845987477,-33.5764163413526,3.01347235406993));
#8827=CARTESIAN_POINT('Ctrl Pts',(-42.8061496104729,-31.839625832053,2.88657884724557));
#8828=CARTESIAN_POINT('Ctrl Pts',(-43.0713229016765,-30.4091655913233,2.81261358016311));
#8829=CARTESIAN_POINT('Ctrl Pts',(-43.0693702153585,-30.0016239406685,2.79157655282254));
#8830=CARTESIAN_POINT('Origin',(-40.,-30.,12.2084234471775));
#8831=CARTESIAN_POINT('',(-43.0746301560641,-29.9972894802837,4.79157655282255));
#8832=CARTESIAN_POINT('',(-43.0703655079321,-30.0022376271458,4.70842344717746));
#8833=CARTESIAN_POINT('',(-43.0735,-29.9999999999999,12.2084234471775));
#8834=CARTESIAN_POINT('Ctrl Pts',(-43.0703655079321,-30.0022376271458,4.70842344717746));
#8835=CARTESIAN_POINT('Ctrl Pts',(-43.0658561305564,-29.3333520268071,4.67386791729991));
#8836=CARTESIAN_POINT('Ctrl Pts',(-42.5219683951878,-27.6332680766331,4.58638414768047));
#8837=CARTESIAN_POINT('Ctrl Pts',(-39.7160732125092,-26.378202307679,4.44597213831914));
#8838=CARTESIAN_POINT('Ctrl Pts',(-36.8029609568071,-28.274608942761,4.28718741909346));
#8839=CARTESIAN_POINT('Ctrl Pts',(-36.8166851325132,-31.7505825885012,4.12840269986777));
#8840=CARTESIAN_POINT('Ctrl Pts',(-39.7446814839369,-33.6239267930437,3.96961798064209));
#8841=CARTESIAN_POINT('Ctrl Pts',(-42.5322369185202,-32.3505540147196,3.82962489641198));
#8842=CARTESIAN_POINT('Ctrl Pts',(-43.0659167364777,-30.6587195938717,3.74256005192377));
#8843=CARTESIAN_POINT('Ctrl Pts',(-43.0701875259343,-29.9978467536557,3.70842344717745));
#8844=CARTESIAN_POINT('Ctrl Pts',(-43.0746301560641,-29.9972894802837,4.79157655282255));
#8845=CARTESIAN_POINT('Ctrl Pts',(-43.0764899884764,-29.794937018229,4.78108579039918));
#8846=CARTESIAN_POINT('Ctrl Pts',(-42.9660572832244,-28.5736912792188,4.71766678823392));
#8847=CARTESIAN_POINT('Ctrl Pts',(-41.3319070183432,-26.6200507172078,4.60131954632676));
#8848=CARTESIAN_POINT('Ctrl Pts',(-37.8823640875572,-27.0481105030832,4.44253482710108));
#8849=CARTESIAN_POINT('Ctrl Pts',(-36.3714818529893,-30.1785763605433,4.28375010787539));
#8850=CARTESIAN_POINT('Ctrl Pts',(-38.1824480418478,-33.1455585099229,4.12496538864971));
#8851=CARTESIAN_POINT('Ctrl Pts',(-41.6573530239065,-33.2328338054134,3.96618066942403));
#8852=CARTESIAN_POINT('Ctrl Pts',(-43.0274482178419,-31.2225585598601,3.85505105748164));
#8853=CARTESIAN_POINT('Ctrl Pts',(-43.0780464961614,-30.1032148835213,3.79684968528114));
#8854=CARTESIAN_POINT('Ctrl Pts',(-43.0773599558693,-30.0017378642629,3.79157655282254));
#8855=CARTESIAN_POINT('Origin',(-40.,-30.,12.2084234471775));
#8856=CARTESIAN_POINT('',(-43.0685124799068,-29.9999333228573,5.79157655282255));
#8857=CARTESIAN_POINT('',(-43.0782646401543,-30.0009171118044,5.70842344717746));
#8858=CARTESIAN_POINT('',(-43.0735,-29.9999999999999,12.2084234471775));
#8859=CARTESIAN_POINT('Ctrl Pts',(-43.0782646401543,-30.0009171118044,5.70842344717746));
#8860=CARTESIAN_POINT('Ctrl Pts',(-43.0744584403933,-29.0333155961755,5.65810402241795));
#8861=CARTESIAN_POINT('Ctrl Pts',(-42.0609602719212,-27.0410775869535,5.55485635791654));
#8862=CARTESIAN_POINT('Ctrl Pts',(-38.6680930076518,-26.6200507831746,5.39868045367324));
#8863=CARTESIAN_POINT('Ctrl Pts',(-36.4378889936663,-29.286278679664,5.23989573444756));
#8864=CARTESIAN_POINT('Ctrl Pts',(-37.4687387628032,-32.6059066548152,5.08111101522187));
#8865=CARTESIAN_POINT('Ctrl Pts',(-40.8169163802229,-33.5398701349496,4.92232629599619));
#8866=CARTESIAN_POINT('Ctrl Pts',(-42.8513292644709,-31.7351429919527,4.79809710664805));
#8867=CARTESIAN_POINT('Ctrl Pts',(-43.0727630831533,-30.357875092727,4.72679615704181));
#8868=CARTESIAN_POINT('Ctrl Pts',(-43.0703655079321,-30.0022376271458,4.70842344717746));
#8869=CARTESIAN_POINT('Ctrl Pts',(-43.0685124799068,-29.9999333228573,5.79157655282255));
#8870=CARTESIAN_POINT('Ctrl Pts',(-43.0686109449675,-29.4909573454998,5.76532189551721));
#8871=CARTESIAN_POINT('Ctrl Pts',(-42.7076775234749,-27.9560394652001,5.68613899846998));
#8872=CARTESIAN_POINT('Ctrl Pts',(-40.2839267930322,-26.378202236992,5.55402786168086));
#8873=CARTESIAN_POINT('Ctrl Pts',(-37.1108841916168,-27.7974915878749,5.39524314245518));
#8874=CARTESIAN_POINT('Ctrl Pts',(-36.5827793869729,-31.2331410063646,5.23645842322949));
#8875=CARTESIAN_POINT('Ctrl Pts',(-39.1830836038332,-33.5398702040376,5.07767370400381));
#8876=CARTESIAN_POINT('Ctrl Pts',(-42.3100502230137,-32.6676128271532,4.9293797472015));
#8877=CARTESIAN_POINT('Ctrl Pts',(-43.0671067185266,-30.8158503886565,4.83401403014107));
#8878=CARTESIAN_POINT('Ctrl Pts',(-43.0746301560641,-29.9972894802837,4.79157655282255));
#8879=CARTESIAN_POINT('Origin',(-40.,-30.,12.2084234471775));
#8880=CARTESIAN_POINT('',(-43.0743853226466,-30.0027445702633,6.79157655282254));
#8881=CARTESIAN_POINT('',(-43.0730720299995,-29.9971906094003,6.70842344717746));
#8882=CARTESIAN_POINT('',(-43.0735,-29.9999999999999,12.2084234471775));
#8883=CARTESIAN_POINT('Ctrl Pts',(-43.0730720299995,-29.9971906094003,6.70842344717746));
#8884=CARTESIAN_POINT('Ctrl Pts',(-43.0753735197904,-29.7431173959859,6.69526836727788));
#8885=CARTESIAN_POINT('Ctrl Pts',(-42.9303369508968,-28.4693960950782,6.6291850476364));
#8886=CARTESIAN_POINT('Ctrl Pts',(-41.1605539334494,-26.5574504348784,6.51017348825302));
#8887=CARTESIAN_POINT('Ctrl Pts',(-37.7368489615224,-27.1581378775489,6.35138876902735));
#8888=CARTESIAN_POINT('Ctrl Pts',(-36.3850213798334,-30.3605031490362,6.19260404980165));
#8889=CARTESIAN_POINT('Ctrl Pts',(-38.3426470084403,-33.2328337423178,6.03381933057598));
#8890=CARTESIAN_POINT('Ctrl Pts',(-41.8175519226788,-33.1455584485307,5.87503461135029));
#8891=CARTESIAN_POINT('Ctrl Pts',(-43.0546166608162,-31.1188232072758,5.76656931688412));
#8892=CARTESIAN_POINT('Ctrl Pts',(-43.0784619729141,-30.0510824971007,5.71103226215984));
#8893=CARTESIAN_POINT('Ctrl Pts',(-43.0782646401543,-30.0009171118044,5.70842344717746));
#8894=CARTESIAN_POINT('Ctrl Pts',(-43.0743853226466,-30.0027445702633,6.79157655282254));
#8895=CARTESIAN_POINT('Ctrl Pts',(-43.0669064799895,-29.1920981213188,6.74955800063525));
#8896=CARTESIAN_POINT('Ctrl Pts',(-42.3222290891344,-27.3481778162171,6.65461120870605));
#8897=CARTESIAN_POINT('Ctrl Pts',(-39.2110615557591,-26.4537894026696,6.50673617703496));
#8898=CARTESIAN_POINT('Ctrl Pts',(-36.592623388795,-28.7399134586708,6.34795145780928));
#8899=CARTESIAN_POINT('Ctrl Pts',(-37.0935822247194,-32.1796259246658,6.18916673858359));
#8900=CARTESIAN_POINT('Ctrl Pts',(-40.2553185210464,-33.623926863772,6.03038201935791));
#8901=CARTESIAN_POINT('Ctrl Pts',(-42.6991780260579,-32.0603354207011,5.89785195743756));
#8902=CARTESIAN_POINT('Ctrl Pts',(-43.0684124437158,-30.5170306337223,5.81825013525911));
#8903=CARTESIAN_POINT('Ctrl Pts',(-43.0685124799068,-29.9999333228573,5.79157655282255));
#8904=CARTESIAN_POINT('Origin',(-40.,-30.,12.2084234471775));
#8905=CARTESIAN_POINT('',(-43.0775324815367,-29.9983795011158,7.79157655282255));
#8906=CARTESIAN_POINT('',(-43.0686901931836,-30.000771834183,7.70842344717745));
#8907=CARTESIAN_POINT('',(-43.0735,-29.9999999999999,12.2084234471775));
#8908=CARTESIAN_POINT('Ctrl Pts',(-43.0686901931836,-30.000771834183,7.70842344717745));
#8909=CARTESIAN_POINT('Ctrl Pts',(-43.0674306982834,-29.4402261026139,7.67950447239591));
#8910=CARTESIAN_POINT('Ctrl Pts',(-42.652072715104,-27.8520175651811,7.59765725787246));
#8911=CARTESIAN_POINT('Ctrl Pts',(-40.1017542238995,-26.368515623773,7.46288180360714));
#8912=CARTESIAN_POINT('Ctrl Pts',(-37.0039607781453,-27.9453024583394,7.30409708438144));
#8913=CARTESIAN_POINT('Ctrl Pts',(-36.6489917431023,-31.4031310114043,7.14531236515577));
#8914=CARTESIAN_POINT('Ctrl Pts',(-39.3618154137075,-33.5764162715476,6.98652764593008));
#8915=CARTESIAN_POINT('Ctrl Pts',(-42.3857290483333,-32.5667565507764,6.84089800660397));
#8916=CARTESIAN_POINT('Ctrl Pts',(-43.0661136897974,-30.7653573256739,6.74819660701977));
#8917=CARTESIAN_POINT('Ctrl Pts',(-43.0730720299995,-29.9971906094003,6.70842344717746));
#8918=CARTESIAN_POINT('Ctrl Pts',(-43.0775324815367,-29.9983795011158,7.79157655282255));
#8919=CARTESIAN_POINT('Ctrl Pts',(-43.0781299166727,-29.904978127604,7.78672234549517));
#8920=CARTESIAN_POINT('Ctrl Pts',(-43.0319030689719,-28.7937668030163,7.72893989842591));
#8921=CARTESIAN_POINT('Ctrl Pts',(-41.6828291578641,-26.7803544372571,7.61822921161475));
#8922=CARTESIAN_POINT('Ctrl Pts',(-38.2073436047123,-26.8401872096979,7.45944449238906));
#8923=CARTESIAN_POINT('Ctrl Pts',(-36.3730050616526,-29.7927767730296,7.30065977316338));
#8924=CARTESIAN_POINT('Ctrl Pts',(-37.8591206231434,-32.9350755877781,7.1418750539377));
#8925=CARTESIAN_POINT('Ctrl Pts',(-41.3051758117063,-33.390361281965,6.98309033471201));
#8926=CARTESIAN_POINT('Ctrl Pts',(-42.9606413632765,-31.4426979504252,6.86632416767362));
#8927=CARTESIAN_POINT('Ctrl Pts',(-43.0763271276925,-30.2132206341649,6.80248624037714));
#8928=CARTESIAN_POINT('Ctrl Pts',(-43.0743853226466,-30.0027445702633,6.79157655282254));
#8929=CARTESIAN_POINT('Origin',(-40.,-30.,12.2084234471775));
#8930=CARTESIAN_POINT('',(-43.069498762849,-29.9982750316902,8.79157655282255));
#8931=CARTESIAN_POINT('',(-43.0759025811495,-30.0024148106623,8.70842344717746));
#8932=CARTESIAN_POINT('',(-43.0735,-29.9999999999999,12.2084234471775));
#8933=CARTESIAN_POINT('Ctrl Pts',(-43.0759025811495,-30.0024148106623,8.70842344717746));
#8934=CARTESIAN_POINT('Ctrl Pts',(-43.0684827561252,-29.1414654488785,8.66374057751394));
#8935=CARTESIAN_POINT('Ctrl Pts',(-42.242973022817,-27.2482214756128,8.56612946810854));
#8936=CARTESIAN_POINT('Ctrl Pts',(-39.0340360123693,-26.4978675466446,8.41559011896124));
#8937=CARTESIAN_POINT('Ctrl Pts',(-36.5336631669943,-28.9125517618253,8.25680539973554));
#8938=CARTESIAN_POINT('Ctrl Pts',(-37.2066641286517,-32.3227807484881,8.09802068050986));
#8939=CARTESIAN_POINT('Ctrl Pts',(-40.4369180883703,-33.6065403909949,7.93923596128418));
#8940=CARTESIAN_POINT('Ctrl Pts',(-42.7517136191364,-31.9560991031317,7.80937021684005));
#8941=CARTESIAN_POINT('Ctrl Pts',(-43.0697358577345,-30.4661510909961,7.7324327121378));
#8942=CARTESIAN_POINT('Ctrl Pts',(-43.0686901931836,-30.000771834183,7.70842344717745));
#8943=CARTESIAN_POINT('Ctrl Pts',(-43.069498762849,-29.9982750316902,8.79157655282255));
#8944=CARTESIAN_POINT('Ctrl Pts',(-43.0715489864528,-29.5988875600661,8.77095845061321));
#8945=CARTESIAN_POINT('Ctrl Pts',(-42.8134919208485,-28.1767814426558,8.69741210866198));
#8946=CARTESIAN_POINT('Ctrl Pts',(-40.6663949208769,-26.4287479717036,8.57093752696886));
#8947=CARTESIAN_POINT('Ctrl Pts',(-37.3607498677919,-27.5035230729969,8.41215280774315));
#8948=CARTESIAN_POINT('Ctrl Pts',(-36.4712752548112,-30.8638056099088,8.25336808851749));
#8949=CARTESIAN_POINT('Ctrl Pts',(-38.8122995967417,-33.4332763392514,8.0945833692918));
#8950=CARTESIAN_POINT('Ctrl Pts',(-42.1358313982743,-32.8771817964379,7.94065285739349));
#8951=CARTESIAN_POINT('Ctrl Pts',(-43.07161573465,-30.9233875106515,7.83965058523707));
#8952=CARTESIAN_POINT('Ctrl Pts',(-43.0775324815367,-29.9983795011158,7.79157655282255));
#8953=CARTESIAN_POINT('Origin',(-40.,-30.,12.2084234471775));
#8954=CARTESIAN_POINT('',(-43.0704010605908,-30.0034624020472,9.79157655282255));
#8955=CARTESIAN_POINT('',(-43.0762856310176,-29.997782176874,9.70842344717746));
#8956=CARTESIAN_POINT('',(-43.0735,-29.9999999999999,12.2084234471775));
#8957=CARTESIAN_POINT('',(-40.7937992825329,-32.9692229537457,10.));
#8958=CARTESIAN_POINT('Ctrl Pts',(-40.7937992825329,-32.9692229537457,10.));
#8959=CARTESIAN_POINT('Ctrl Pts',(-41.7812379463276,-32.7052387009375,9.94707176025811));
#8960=CARTESIAN_POINT('Ctrl Pts',(-42.879629843998,-31.663795760744,9.87759727786561));
#8961=CARTESIAN_POINT('Ctrl Pts',(-43.072821611806,-30.3235455230037,9.80812279547314));
#8962=CARTESIAN_POINT('Ctrl Pts',(-43.0704010605908,-30.0034624020472,9.79157655282255));
#8963=CARTESIAN_POINT('',(-39.204453684107,-32.9745272669182,10.));
#8964=CARTESIAN_POINT('Origin',(-40.,-30.,10.));
#8965=CARTESIAN_POINT('Ctrl Pts',(-39.2044522699742,-32.9745315604842,10.));
#8966=CARTESIAN_POINT('Ctrl Pts',(-40.166639343954,-33.2303406669821,9.94821753066412));
#8967=CARTESIAN_POINT('Ctrl Pts',(-42.2305616481375,-32.7556949590643,9.85102534638995));
#8968=CARTESIAN_POINT('Ctrl Pts',(-43.0690540701593,-30.8722543038914,9.75383316211577));
#8969=CARTESIAN_POINT('Ctrl Pts',(-43.0762856310176,-29.997782176874,9.70842344717746));
#8970=CARTESIAN_POINT('Origin',(-40.,-30.,12.2084234471775));
#8971=CARTESIAN_POINT('Ctrl Pts',(-43.0762856310176,-29.997782176874,9.70842344717746));
#8972=CARTESIAN_POINT('Ctrl Pts',(-43.0774829666484,-29.852995089222,9.70090492237387));
#8973=CARTESIAN_POINT('Ctrl Pts',(-43.0023605019912,-28.6901611816683,9.64045815782839));
#8974=CARTESIAN_POINT('Ctrl Pts',(-41.5191024081009,-26.6996618460447,9.52708315354101));
#8975=CARTESIAN_POINT('Ctrl Pts',(-38.0509701816934,-26.934299866359,9.36829843431533));
#8976=CARTESIAN_POINT('Ctrl Pts',(-36.3671808918873,-29.9750448667934,9.20951371508965));
#8977=CARTESIAN_POINT('Ctrl Pts',(-38.0091582883336,-33.0388816507496,9.05072899586396));
#8978=CARTESIAN_POINT('Ctrl Pts',(-41.4737279965523,-33.3205494224222,8.89194427663828));
#8979=CARTESIAN_POINT('Ctrl Pts',(-42.9938368358631,-31.3385369294681,8.77784242707611));
#8980=CARTESIAN_POINT('Ctrl Pts',(-43.0772717681266,-30.1612865697975,8.71666881725583));
#8981=CARTESIAN_POINT('Ctrl Pts',(-43.0759025811495,-30.0024148106623,8.70842344717746));
#8982=CARTESIAN_POINT('Ctrl Pts',(-43.0704010605908,-30.0034624020472,9.79157655282255));
#8983=CARTESIAN_POINT('Ctrl Pts',(-43.0650787352067,-29.2996613384747,9.75519455573124));
#8984=CARTESIAN_POINT('Ctrl Pts',(-42.4772114414296,-27.5614694578342,9.66588431889805));
#8985=CARTESIAN_POINT('Ctrl Pts',(-39.5908856218057,-26.3909740388041,9.52364584232295));
#8986=CARTESIAN_POINT('Ctrl Pts',(-36.745809981275,-28.3852514028181,9.36486112309727));
#8987=CARTESIAN_POINT('Ctrl Pts',(-36.8786561820279,-31.8593324073604,9.20607640387158));
#8988=CARTESIAN_POINT('Ctrl Pts',(-39.869659454766,-33.6304609478428,9.0472916846459));
#8989=CARTESIAN_POINT('Ctrl Pts',(-42.5758437009482,-32.2798864461415,8.90912506762956));
#8990=CARTESIAN_POINT('Ctrl Pts',(-43.0662859062079,-30.6241456383026,8.8238866903551));
#8991=CARTESIAN_POINT('Ctrl Pts',(-43.069498762849,-29.9982750316902,8.79157655282255));
#8992=CARTESIAN_POINT('Ctrl Pts',(-38.0865340033349,-28.364012796625,10.));
#8993=CARTESIAN_POINT('Ctrl Pts',(-37.5424734719262,-29.0003511034471,9.94707176025811));
#8994=CARTESIAN_POINT('Ctrl Pts',(-37.1490030310892,-30.8479858487614,9.84121528077432));
#8995=CARTESIAN_POINT('Ctrl Pts',(-39.1694205041011,-32.8592860233099,9.68243056154863));
#8996=CARTESIAN_POINT('Ctrl Pts',(-41.9506458901437,-32.2463502392111,9.52364584232295));
#8997=CARTESIAN_POINT('Ctrl Pts',(-42.9458435562516,-29.5801375894759,9.36486112309726));
#8998=CARTESIAN_POINT('Ctrl Pts',(-41.2442948795815,-27.2966971522426,9.20607640387158));
#8999=CARTESIAN_POINT('Ctrl Pts',(-38.4035521172648,-27.4888888607642,9.0472916846459));
#9000=CARTESIAN_POINT('Ctrl Pts',(-37.0243624191724,-29.9795592816503,8.88850696542021));
#9001=CARTESIAN_POINT('Ctrl Pts',(-38.3693040477892,-32.4891441534934,8.72972224619453));
#9002=CARTESIAN_POINT('Ctrl Pts',(-41.2071287559201,-32.7198578724412,8.57093752696884));
#9003=CARTESIAN_POINT('Ctrl Pts',(-42.9398430866436,-30.460637110478,8.41215280774317));
#9004=CARTESIAN_POINT('Ctrl Pts',(-41.9811816092491,-27.779685411444,8.25336808851748));
#9005=CARTESIAN_POINT('Ctrl Pts',(-39.2087801077402,-27.1314076943803,8.0945833692918));
#9006=CARTESIAN_POINT('Ctrl Pts',(-37.1607278421696,-29.1092725102961,7.93579865006611));
#9007=CARTESIAN_POINT('Ctrl Pts',(-37.7119820868328,-31.9025868014703,7.77701393084044));
#9008=CARTESIAN_POINT('Ctrl Pts',(-40.3578790588815,-32.9541127165542,7.61822921161474));
#9009=CARTESIAN_POINT('Ctrl Pts',(-42.6761436022691,-31.3011980345695,7.45944449238907));
#9010=CARTESIAN_POINT('Ctrl Pts',(-42.5444429166006,-28.4570576484011,7.30065977316337));
#9011=CARTESIAN_POINT('Ctrl Pts',(-40.0833467573344,-27.025455696388,7.1418750539377));
#9012=CARTESIAN_POINT('Ctrl Pts',(-37.5459480263481,-28.3169998174294,6.98309033471201));
#9013=CARTESIAN_POINT('Ctrl Pts',(-37.255193334394,-31.1493028538182,6.82430561548633));
#9014=CARTESIAN_POINT('Ctrl Pts',(-39.4772638047856,-32.9294380880498,6.66552089626065));
#9015=CARTESIAN_POINT('Ctrl Pts',(-42.1778906257405,-32.0277211571395,6.50673617703496));
#9016=CARTESIAN_POINT('Ctrl Pts',(-42.8846945563006,-29.2696589968946,6.34795145780928));
#9017=CARTESIAN_POINT('Ctrl Pts',(-40.950608273128,-27.1802119634965,6.18916673858359));
#9018=CARTESIAN_POINT('Ctrl Pts',(-38.1462558193046,-27.6722342953406,6.03038201935791));
#9019=CARTESIAN_POINT('Ctrl Pts',(-37.0389755405013,-30.2952876777936,5.87159730013223));
#9020=CARTESIAN_POINT('Ctrl Pts',(-38.642464240686,-32.6480100687441,5.71281258090654));
#9021=CARTESIAN_POINT('Ctrl Pts',(-41.4887545031215,-32.5765229849279,5.55402786168087));
#9022=CARTESIAN_POINT('Ctrl Pts',(-42.9721146109695,-30.1462716703736,5.39524314245517));
#9023=CARTESIAN_POINT('Ctrl Pts',(-41.7345528893855,-27.5821110579311,5.2364584232295));
#9024=CARTESIAN_POINT('Ctrl Pts',(-38.9090366509723,-27.2314878303699,5.07767370400381));
#9025=CARTESIAN_POINT('Ctrl Pts',(-37.0822793367675,-29.4153917605512,4.91888898477813));
#9026=CARTESIAN_POINT('Ctrl Pts',(-37.9266470913801,-32.134494876687,4.76010426555244));
#9027=CARTESIAN_POINT('Ctrl Pts',(-40.6691351837356,-32.8995031933417,4.60131954632676));
#9028=CARTESIAN_POINT('Ctrl Pts',(-42.7990410689418,-31.0100642339135,4.44253482710107));
#9029=CARTESIAN_POINT('Ctrl Pts',(-42.3664710934277,-28.1959281537966,4.28375010787539));
#9030=CARTESIAN_POINT('Ctrl Pts',(-39.7674359240253,-27.0333900470415,4.12496538864971));
#9031=CARTESIAN_POINT('Ctrl Pts',(-37.3813093244711,-28.5867343463155,3.96618066942403));
#9032=CARTESIAN_POINT('Ctrl Pts',(-37.3925507796004,-31.4339000053853,3.80739595019834));
#9033=CARTESIAN_POINT('Ctrl Pts',(-39.7908689233158,-32.9683538966935,3.64861123097266));
#9034=CARTESIAN_POINT('Ctrl Pts',(-42.3806431125633,-31.7853288297545,3.48982651174697));
#9035=CARTESIAN_POINT('Ctrl Pts',(-42.7909778595383,-28.9678647125816,3.33104179252129));
#9036=CARTESIAN_POINT('Ctrl Pts',(-40.646218478806,-27.0953033985544,3.17225707329561));
#9037=CARTESIAN_POINT('Ctrl Pts',(-37.9098567596893,-27.881943844822,3.01347235406992));
#9038=CARTESIAN_POINT('Ctrl Pts',(-37.0869866417049,-30.6076297028158,2.85468763484424));
#9039=CARTESIAN_POINT('Ctrl Pts',(-38.9309321484219,-32.777040624953,2.69590291561856));
#9040=CARTESIAN_POINT('Ctrl Pts',(-41.7535915815893,-32.4041166904058,2.53711819639287));
#9041=CARTESIAN_POINT('Ctrl Pts',(-42.9708669527046,-29.830263717713,2.37833347716719));
#9042=CARTESIAN_POINT('Ctrl Pts',(-41.4683625791277,-27.4118013520306,2.21954875794151));
#9043=CARTESIAN_POINT('Ctrl Pts',(-38.621596771745,-27.3627924042219,2.06076403871582));
#9044=CARTESIAN_POINT('Ctrl Pts',(-37.0367358479852,-29.7281028255258,1.90197931949014));
#9045=CARTESIAN_POINT('Ctrl Pts',(-38.1646953067422,-32.3423318573701,1.74319460026445));
#9046=CARTESIAN_POINT('Ctrl Pts',(-40.9728438931775,-32.812192293083,1.58440988103877));
#9047=CARTESIAN_POINT('Ctrl Pts',(-42.8903739628085,-30.707542080798,1.42562516181309));
#9048=CARTESIAN_POINT('Ctrl Pts',(-42.1618064338936,-27.9551389132726,1.2668404425874));
#9049=CARTESIAN_POINT('Ctrl Pts',(-39.454156767702,-27.0747919996342,1.10805572336172));
#9050=CARTESIAN_POINT('Ctrl Pts',(-37.2461857259263,-28.8723853276339,0.949271004136036));
#9051=CARTESIAN_POINT('Ctrl Pts',(-37.5593497462198,-31.7023698699528,0.790486284910354));
#9052=CARTESIAN_POINT('Ctrl Pts',(-40.1067617676959,-32.9737059237326,0.63170156568467));
#9053=CARTESIAN_POINT('Ctrl Pts',(-42.5566887710618,-31.5229768750616,0.472916846458986));
#9054=CARTESIAN_POINT('Ctrl Pts',(-42.6655029077533,-28.6773613681587,0.314132127233303));
#9055=CARTESIAN_POINT('Ctrl Pts',(-40.3351050630486,-27.0438515966452,0.155347408007618));
#9056=CARTESIAN_POINT('Ctrl Pts',(-37.6958995373424,-28.1141315210005,-0.00343731121806404));
#9057=CARTESIAN_POINT('Ctrl Pts',(-37.1701534642436,-30.9160962288461,-0.162222030443749));
#9058=CARTESIAN_POINT('Ctrl Pts',(-38.5409902294193,-32.2158576312381,-0.268078509927538));
#9059=CARTESIAN_POINT('Ctrl Pts',(-39.3498000020249,-32.4320868020351,-0.321006749669432));
#9060=CARTESIAN_POINT('Ctrl Pts',(-37.9456684496579,-28.2435746787731,10.1070022498898));
#9061=CARTESIAN_POINT('Ctrl Pts',(-37.3615552660859,-28.9267589437008,10.0540740101479));
#9062=CARTESIAN_POINT('Ctrl Pts',(-36.9391183154699,-30.9104128771509,9.94821753066413));
#9063=CARTESIAN_POINT('Ctrl Pts',(-39.1082748967234,-33.0697809625963,9.78943281143844));
#9064=CARTESIAN_POINT('Ctrl Pts',(-42.0942485534896,-32.41172206748,9.63064809221276));
#9065=CARTESIAN_POINT('Ctrl Pts',(-43.1627106886284,-29.5492281554804,9.47186337298707));
#9066=CARTESIAN_POINT('Ctrl Pts',(-41.335897389088,-27.09768538351,9.3130786537614));
#9067=CARTESIAN_POINT('Ctrl Pts',(-38.2860248054076,-27.3040258626292,9.1542939345357));
#9068=CARTESIAN_POINT('Ctrl Pts',(-36.8053019100774,-29.978054476698,8.99550921531003));
#9069=CARTESIAN_POINT('Ctrl Pts',(-38.249255461304,-32.6723899859121,8.83672449608433));
#9070=CARTESIAN_POINT('Ctrl Pts',(-41.2959951694642,-32.9200883891015,8.67793977685867));
#9071=CARTESIAN_POINT('Ctrl Pts',(-43.1562684764051,-30.4945482966316,8.51915505763297));
#9072=CARTESIAN_POINT('Ctrl Pts',(-42.1270322513865,-27.6162302758946,8.36037033840729));
#9073=CARTESIAN_POINT('Ctrl Pts',(-39.1505320759499,-26.920227645135,8.20158561918161));
#9074=CARTESIAN_POINT('Ctrl Pts',(-36.9517062837778,-29.0436989274726,8.04280089995592));
#9075=CARTESIAN_POINT('Ctrl Pts',(-37.5435427674391,-32.0426514504762,7.88401618073024));
#9076=CARTESIAN_POINT('Ctrl Pts',(-40.3842254020444,-33.1715886080345,7.72523146150456));
#9077=CARTESIAN_POINT('Ctrl Pts',(-42.8731559614695,-31.3969896409542,7.56644674227887));
#9078=CARTESIAN_POINT('Ctrl Pts',(-42.7317597337645,-28.3434693071248,7.40766202305319));
#9079=CARTESIAN_POINT('Ctrl Pts',(-40.0894825795227,-26.806475672183,7.24887730382751));
#9080=CARTESIAN_POINT('Ctrl Pts',(-37.3652856102805,-28.1931006977328,7.09009258460182));
#9081=CARTESIAN_POINT('Ctrl Pts',(-37.0531261372968,-31.2339122396802,6.93130786537614));
#9082=CARTESIAN_POINT('Ctrl Pts',(-39.4387810077596,-33.145097482549,6.77252314615045));
#9083=CARTESIAN_POINT('Ctrl Pts',(-42.3382225936864,-32.1769979480524,6.61373842692477));
#9084=CARTESIAN_POINT('Ctrl Pts',(-43.0970600211537,-29.2158927476094,6.45495370769909));
#9085=CARTESIAN_POINT('Ctrl Pts',(-41.0205901599018,-26.9726247872904,6.29616898847341));
#9086=CARTESIAN_POINT('Ctrl Pts',(-38.0097868667106,-27.5008688227433,6.13738426924772));
#9087=CARTESIAN_POINT('Ctrl Pts',(-36.8209908202787,-30.3170261682078,5.97859955002204));
#9088=CARTESIAN_POINT('Ctrl Pts',(-38.5425251632707,-32.8429512932687,5.81981483079635));
#9089=CARTESIAN_POINT('Ctrl Pts',(-41.598353642974,-32.7662014727955,5.66103011157068));
#9090=CARTESIAN_POINT('Ctrl Pts',(-43.1909157660438,-30.1570398992684,5.50224539234498));
#9091=CARTESIAN_POINT('Ctrl Pts',(-41.8622472166279,-27.4041108921859,5.34346067311931));
#9092=CARTESIAN_POINT('Ctrl Pts',(-38.8287221031988,-27.0276754813048,5.18467595389362));
#9093=CARTESIAN_POINT('Ctrl Pts',(-36.8674825557338,-29.3723540669221,5.02589123466794));
#9094=CARTESIAN_POINT('Ctrl Pts',(-37.7740109818545,-32.291632136063,4.86710651544225));
#9095=CARTESIAN_POINT('Ctrl Pts',(-40.7183955825647,-33.1129588405443,4.70832179621657));
#9096=CARTESIAN_POINT('Ctrl Pts',(-43.0051008947389,-31.0844231500414,4.54953707699088));
#9097=CARTESIAN_POINT('Ctrl Pts',(-42.5406859796171,-28.0631159794849,4.3907523577652));
#9098=CARTESIAN_POINT('Ctrl Pts',(-39.7503150201867,-26.8149941339207,4.23196763853952));
#9099=CARTESIAN_POINT('Ctrl Pts',(-37.1885265352497,-28.4826925451306,4.07318291931384));
#9100=CARTESIAN_POINT('Ctrl Pts',(-37.2005955639047,-31.5394608664239,3.91439820008815));
#9101=CARTESIAN_POINT('Ctrl Pts',(-39.7754731101895,-33.1868781954769,3.75561348086247));
#9102=CARTESIAN_POINT('Ctrl Pts',(-42.5559013145607,-31.9167611805448,3.59682876163678));
#9103=CARTESIAN_POINT('Ctrl Pts',(-42.9964440879267,-28.891880969476,3.4380440424111));
#9104=CARTESIAN_POINT('Ctrl Pts',(-40.6937917954847,-26.8814654229962,3.27925932318542));
#9105=CARTESIAN_POINT('Ctrl Pts',(-37.755984579403,-27.7260167713657,3.12047460395974));
#9106=CARTESIAN_POINT('Ctrl Pts',(-36.8725364030803,-30.6523621907026,2.96168988473405));
#9107=CARTESIAN_POINT('Ctrl Pts',(-38.8522295035391,-32.9814808219043,2.80290516550837));
#9108=CARTESIAN_POINT('Ctrl Pts',(-41.8826874994131,-32.5811029704277,2.64412044628268));
#9109=CARTESIAN_POINT('Ctrl Pts',(-43.1895762576637,-29.8177680708476,2.485335727057));
#9110=CARTESIAN_POINT('Ctrl Pts',(-41.5764605061711,-27.2212633251162,2.32655100783131));
#9111=CARTESIAN_POINT('Ctrl Pts',(-38.5201214728493,-27.1686464362308,2.16776628860563));
#9112=CARTESIAN_POINT('Ctrl Pts',(-36.8185862460626,-29.7080862973553,2.00898156937995));
#9113=CARTESIAN_POINT('Ctrl Pts',(-38.0295838324686,-32.5147696611037,1.85019685015426));
#9114=CARTESIAN_POINT('Ctrl Pts',(-41.0444627219901,-33.0192202857946,1.69141213092858));
#9115=CARTESIAN_POINT('Ctrl Pts',(-43.1031575342513,-30.7596299188548,1.5326274117029));
#9116=CARTESIAN_POINT('Ctrl Pts',(-42.3209543156871,-27.8046003148985,1.37384269247721));
#9117=CARTESIAN_POINT('Ctrl Pts',(-39.4139728766517,-26.8594440157609,1.21505797325153));
#9118=CARTESIAN_POINT('Ctrl Pts',(-37.0434554066433,-28.789372582472,1.05627325402585));
#9119=CARTESIAN_POINT('Ctrl Pts',(-37.3796739380633,-31.8276949474362,0.897488534800165));
#9120=CARTESIAN_POINT('Ctrl Pts',(-40.1146213562876,-33.1926242280815,0.738703815574481));
#9121=CARTESIAN_POINT('Ctrl Pts',(-42.7449071036286,-31.6350953977407,0.579919096348796));
#9122=CARTESIAN_POINT('Ctrl Pts',(-42.8617319202273,-28.5799913477279,0.421134377123115));
#9123=CARTESIAN_POINT('Ctrl Pts',(-40.3597748300205,-26.8262258419593,0.262349657897428));
#9124=CARTESIAN_POINT('Ctrl Pts',(-37.5262762527031,-27.9752976415799,0.103564938671747));
#9125=CARTESIAN_POINT('Ctrl Pts',(-36.9618258013664,-30.9835374076926,-0.0552197805539386));
#9126=CARTESIAN_POINT('Ctrl Pts',(-38.4335808375037,-32.3789846544712,-0.161076260037727));
#9127=CARTESIAN_POINT('Ctrl Pts',(-39.301933573839,-32.6111321859386,-0.214004499779622));
#9128=CARTESIAN_POINT('Ctrl Pts',(-37.8048028959809,-28.1231365609212,10.2140044997796));
#9129=CARTESIAN_POINT('Ctrl Pts',(-37.1806370602456,-28.8531667839546,10.1610762600377));
#9130=CARTESIAN_POINT('Ctrl Pts',(-36.7292335998507,-30.9728399055403,10.0552197805539));
#9131=CARTESIAN_POINT('Ctrl Pts',(-39.0471292893458,-33.2802759018827,9.89643506132826));
#9132=CARTESIAN_POINT('Ctrl Pts',(-42.2378512168355,-32.577093895749,9.73765034210256));
#9133=CARTESIAN_POINT('Ctrl Pts',(-43.3795778210052,-29.5183187214848,9.5788656228769));
#9134=CARTESIAN_POINT('Ctrl Pts',(-41.4274998985944,-26.8986736147774,9.4200809036512));
#9135=CARTESIAN_POINT('Ctrl Pts',(-38.1684974935506,-27.1191628644941,9.26129618442552));
#9136=CARTESIAN_POINT('Ctrl Pts',(-36.5862414009823,-29.9765496717457,9.10251146519984));
#9137=CARTESIAN_POINT('Ctrl Pts',(-38.1292068748188,-32.8556358183309,8.94372674597415));
#9138=CARTESIAN_POINT('Ctrl Pts',(-41.3848615830082,-33.1203189057619,8.78494202674847));
#9139=CARTESIAN_POINT('Ctrl Pts',(-43.3726938661667,-30.5284594827854,8.6261573075228));
#9140=CARTESIAN_POINT('Ctrl Pts',(-42.2728828935239,-27.4527751403451,8.4673725882971));
#9141=CARTESIAN_POINT('Ctrl Pts',(-39.0922840441595,-26.7090475958899,8.30858786907142));
#9142=CARTESIAN_POINT('Ctrl Pts',(-36.7426847253861,-28.9781253446489,8.14980314984574));
#9143=CARTESIAN_POINT('Ctrl Pts',(-37.3751034480454,-32.1827160994822,7.99101843062005));
#9144=CARTESIAN_POINT('Ctrl Pts',(-40.4105717452074,-33.3890644995146,7.83223371139437));
#9145=CARTESIAN_POINT('Ctrl Pts',(-43.07016832067,-31.492781247339,7.67344899216868));
#9146=CARTESIAN_POINT('Ctrl Pts',(-42.9190765509283,-28.2298809658486,7.514664272943));
#9147=CARTESIAN_POINT('Ctrl Pts',(-40.0956184017111,-26.587495647978,7.35587955371732));
#9148=CARTESIAN_POINT('Ctrl Pts',(-37.1846231942129,-28.0692015780361,7.19709483449163));
#9149=CARTESIAN_POINT('Ctrl Pts',(-36.8510589401995,-31.3185216255423,7.03831011526596));
#9150=CARTESIAN_POINT('Ctrl Pts',(-39.4002982107335,-33.3607568770483,6.87952539604026));
#9151=CARTESIAN_POINT('Ctrl Pts',(-42.4985545616324,-32.3262747389653,6.72074067681459));
#9152=CARTESIAN_POINT('Ctrl Pts',(-43.3094254860068,-29.1621264983242,6.56195595758889));
#9153=CARTESIAN_POINT('Ctrl Pts',(-41.0905720466756,-26.7650376110844,6.40317123836323));
#9154=CARTESIAN_POINT('Ctrl Pts',(-37.8733179141165,-27.3295033501461,6.24438651913752));
#9155=CARTESIAN_POINT('Ctrl Pts',(-36.6030061000561,-30.338764658622,6.08560179991185));
#9156=CARTESIAN_POINT('Ctrl Pts',(-38.4425860858555,-33.0378925177933,5.92681708068616));
#9157=CARTESIAN_POINT('Ctrl Pts',(-41.7079527828264,-32.9558799606631,5.76803236146049));
#9158=CARTESIAN_POINT('Ctrl Pts',(-43.4097169211181,-30.1678081281632,5.60924764223479));
#9159=CARTESIAN_POINT('Ctrl Pts',(-41.9899415438703,-27.2261107264408,5.45046292300912));
#9160=CARTESIAN_POINT('Ctrl Pts',(-38.7484075554253,-26.8238631322397,5.29167820378342));
#9161=CARTESIAN_POINT('Ctrl Pts',(-36.6526857747,-29.3293163732931,5.13289348455775));
#9162=CARTESIAN_POINT('Ctrl Pts',(-37.6213748723289,-32.4487693954391,4.97410876533206));
#9163=CARTESIAN_POINT('Ctrl Pts',(-40.7676559813938,-33.326414487747,4.81532404610638));
#9164=CARTESIAN_POINT('Ctrl Pts',(-43.2111607205359,-31.1587820661693,4.65653932688069));
#9165=CARTESIAN_POINT('Ctrl Pts',(-42.7149008658065,-27.9303038051732,4.49775460765502));
#9166=CARTESIAN_POINT('Ctrl Pts',(-39.733194116348,-26.5965982207998,4.33896988842933));
#9167=CARTESIAN_POINT('Ctrl Pts',(-36.9957437460284,-28.3786507439458,4.18018516920365));
#9168=CARTESIAN_POINT('Ctrl Pts',(-37.0086403482089,-31.6450217274626,4.02140044997796));
#9169=CARTESIAN_POINT('Ctrl Pts',(-39.7600772970632,-33.4054024942603,3.86261573075228));
#9170=CARTESIAN_POINT('Ctrl Pts',(-42.7311595165581,-32.0481935313351,3.70383101152659));
#9171=CARTESIAN_POINT('Ctrl Pts',(-43.201910316315,-28.8158972263705,3.54504629230092));
#9172=CARTESIAN_POINT('Ctrl Pts',(-40.7413651121635,-26.6676274474379,3.38626157307523));
#9173=CARTESIAN_POINT('Ctrl Pts',(-37.6021123991165,-27.5700896979093,3.22747685384955));
#9174=CARTESIAN_POINT('Ctrl Pts',(-36.6580861644558,-30.6970946785895,3.06869213462386));
#9175=CARTESIAN_POINT('Ctrl Pts',(-38.7735268586563,-33.1859210188555,2.90990741539818));
#9176=CARTESIAN_POINT('Ctrl Pts',(-42.0117834172368,-32.7580892504496,2.7511226961725));
#9177=CARTESIAN_POINT('Ctrl Pts',(-43.4082855626228,-29.805272423982,2.59233797694681));
#9178=CARTESIAN_POINT('Ctrl Pts',(-41.6845584332144,-27.0307252982018,2.43355325772113));
#9179=CARTESIAN_POINT('Ctrl Pts',(-38.4186461739536,-26.9745004682398,2.27476853849544));
#9180=CARTESIAN_POINT('Ctrl Pts',(-36.6004366441401,-29.6880697691848,2.11598381926976));
#9181=CARTESIAN_POINT('Ctrl Pts',(-37.894472358195,-32.6872074648372,1.95719910004408));
#9182=CARTESIAN_POINT('Ctrl Pts',(-41.1160815508026,-33.2262482785062,1.79841438081839));
#9183=CARTESIAN_POINT('Ctrl Pts',(-43.315941105694,-30.8117177569115,1.63962966159271));
#9184=CARTESIAN_POINT('Ctrl Pts',(-42.4801021974805,-27.6540617165245,1.48084494236703));
#9185=CARTESIAN_POINT('Ctrl Pts',(-39.3737889856013,-26.6440960318875,1.32206022314134));
#9186=CARTESIAN_POINT('Ctrl Pts',(-36.8407250873603,-28.7063598373101,1.16327550391566));
#9187=CARTESIAN_POINT('Ctrl Pts',(-37.1999981299068,-31.9530200249197,1.00449078468997));
#9188=CARTESIAN_POINT('Ctrl Pts',(-40.1224809448793,-33.4115425324305,0.845706065464292));
#9189=CARTESIAN_POINT('Ctrl Pts',(-42.9331254361953,-31.7472139204198,0.686921346238607));
#9190=CARTESIAN_POINT('Ctrl Pts',(-43.0579609327015,-28.4826213272971,0.528136627012925));
#9191=CARTESIAN_POINT('Ctrl Pts',(-40.3844445969923,-26.6086000872734,0.369351907787239));
#9192=CARTESIAN_POINT('Ctrl Pts',(-37.3566529680639,-27.8364637621594,0.210567188561558));
#9193=CARTESIAN_POINT('Ctrl Pts',(-36.7534981384891,-31.0509785865391,0.0517824693358723));
#9194=CARTESIAN_POINT('Ctrl Pts',(-38.326171445588,-32.5421116777044,-0.0540740101479163));
#9195=CARTESIAN_POINT('Ctrl Pts',(-39.2540671456531,-32.7901775698422,-0.107002249889811));
#9196=CARTESIAN_POINT('Ctrl Pts',(-37.6639373423038,-28.0026984430693,10.3210067496694));
#9197=CARTESIAN_POINT('Ctrl Pts',(-36.9997188544053,-28.7795746242084,10.2680785099275));
#9198=CARTESIAN_POINT('Ctrl Pts',(-36.5193488842315,-31.0352669339298,10.1622220304438));
#9199=CARTESIAN_POINT('Ctrl Pts',(-38.9859836819681,-33.490770841169,10.0034373112181));
#9200=CARTESIAN_POINT('Ctrl Pts',(-42.3814538801814,-32.7424657240179,9.84465259199238));
#9201=CARTESIAN_POINT('Ctrl Pts',(-43.596444953382,-29.4874092874893,9.6858678727667));
#9202=CARTESIAN_POINT('Ctrl Pts',(-41.5191024081009,-26.6996618460447,9.52708315354101));
#9203=CARTESIAN_POINT('Ctrl Pts',(-38.0509701816934,-26.934299866359,9.36829843431533));
#9204=CARTESIAN_POINT('Ctrl Pts',(-36.3671808918873,-29.9750448667934,9.20951371508965));
#9205=CARTESIAN_POINT('Ctrl Pts',(-38.0091582883336,-33.0388816507496,9.05072899586396));
#9206=CARTESIAN_POINT('Ctrl Pts',(-41.4737279965523,-33.3205494224222,8.89194427663828));
#9207=CARTESIAN_POINT('Ctrl Pts',(-43.5891192559282,-30.562370668939,8.73315955741259));
#9208=CARTESIAN_POINT('Ctrl Pts',(-42.4187335356612,-27.2893200047958,8.57437483818692));
#9209=CARTESIAN_POINT('Ctrl Pts',(-39.0340360123693,-26.4978675466446,8.41559011896124));
#9210=CARTESIAN_POINT('Ctrl Pts',(-36.5336631669943,-28.9125517618253,8.25680539973554));
#9211=CARTESIAN_POINT('Ctrl Pts',(-37.2066641286517,-32.3227807484881,8.09802068050986));
#9212=CARTESIAN_POINT('Ctrl Pts',(-40.4369180883703,-33.6065403909949,7.93923596128418));
#9213=CARTESIAN_POINT('Ctrl Pts',(-43.2671806798705,-31.5885728537237,7.7804512420585));
#9214=CARTESIAN_POINT('Ctrl Pts',(-43.1063933680922,-28.1162926245723,7.62166652283281));
#9215=CARTESIAN_POINT('Ctrl Pts',(-40.1017542238995,-26.368515623773,7.46288180360714));
#9216=CARTESIAN_POINT('Ctrl Pts',(-37.0039607781453,-27.9453024583394,7.30409708438144));
#9217=CARTESIAN_POINT('Ctrl Pts',(-36.6489917431023,-31.4031310114043,7.14531236515577));
#9218=CARTESIAN_POINT('Ctrl Pts',(-39.3618154137075,-33.5764162715476,6.98652764593008));
#9219=CARTESIAN_POINT('Ctrl Pts',(-42.6588865295783,-32.4755515298782,6.82774292670439));
#9220=CARTESIAN_POINT('Ctrl Pts',(-43.5217909508599,-29.1083602490389,6.66895820747872));
#9221=CARTESIAN_POINT('Ctrl Pts',(-41.1605539334494,-26.5574504348784,6.51017348825302));
#9222=CARTESIAN_POINT('Ctrl Pts',(-37.7368489615224,-27.1581378775489,6.35138876902735));
#9223=CARTESIAN_POINT('Ctrl Pts',(-36.3850213798334,-30.3605031490362,6.19260404980165));
#9224=CARTESIAN_POINT('Ctrl Pts',(-38.3426470084403,-33.2328337423178,6.03381933057598));
#9225=CARTESIAN_POINT('Ctrl Pts',(-41.8175519226788,-33.1455584485307,5.87503461135029));
#9226=CARTESIAN_POINT('Ctrl Pts',(-43.6285180761925,-30.1785763570579,5.71624989212461));
#9227=CARTESIAN_POINT('Ctrl Pts',(-42.1176358711127,-27.0481105606956,5.55746517289893));
#9228=CARTESIAN_POINT('Ctrl Pts',(-38.6680930076518,-26.6200507831746,5.39868045367324));
#9229=CARTESIAN_POINT('Ctrl Pts',(-36.4378889936663,-29.286278679664,5.23989573444756));
#9230=CARTESIAN_POINT('Ctrl Pts',(-37.4687387628032,-32.6059066548152,5.08111101522187));
#9231=CARTESIAN_POINT('Ctrl Pts',(-40.8169163802229,-33.5398701349496,4.92232629599619));
#9232=CARTESIAN_POINT('Ctrl Pts',(-43.4172205463328,-31.2331409822972,4.76354157677051));
#9233=CARTESIAN_POINT('Ctrl Pts',(-42.889115751996,-27.7974916308615,4.60475685754482));
#9234=CARTESIAN_POINT('Ctrl Pts',(-39.7160732125092,-26.378202307679,4.44597213831914));
#9235=CARTESIAN_POINT('Ctrl Pts',(-36.8029609568071,-28.274608942761,4.28718741909346));
#9236=CARTESIAN_POINT('Ctrl Pts',(-36.8166851325132,-31.7505825885012,4.12840269986777));
#9237=CARTESIAN_POINT('Ctrl Pts',(-39.7446814839369,-33.6239267930437,3.96961798064209));
#9238=CARTESIAN_POINT('Ctrl Pts',(-42.9064177185554,-32.1796258821253,3.8108332614164));
#9239=CARTESIAN_POINT('Ctrl Pts',(-43.4073765447034,-28.7399134832649,3.65204854219072));
#9240=CARTESIAN_POINT('Ctrl Pts',(-40.7889384288422,-26.4537894718797,3.49326382296504));
#9241=CARTESIAN_POINT('Ctrl Pts',(-37.4482402188302,-27.414162624453,3.33447910373936));
#9242=CARTESIAN_POINT('Ctrl Pts',(-36.4436359258312,-30.7418271664764,3.17569438451367));
#9243=CARTESIAN_POINT('Ctrl Pts',(-38.6948242137735,-33.3903612158066,3.01690966528799));
#9244=CARTESIAN_POINT('Ctrl Pts',(-42.1408793350605,-32.9350755304716,2.85812494606231));
#9245=CARTESIAN_POINT('Ctrl Pts',(-43.6269948675819,-29.7927767771166,2.69934022683662));
#9246=CARTESIAN_POINT('Ctrl Pts',(-41.7926563602578,-26.8401872712874,2.54055550761094));
#9247=CARTESIAN_POINT('Ctrl Pts',(-38.3171708750578,-26.7803545002487,2.38177078838525));
#9248=CARTESIAN_POINT('Ctrl Pts',(-36.3822870422175,-29.6680532410143,2.22298606915957));
#9249=CARTESIAN_POINT('Ctrl Pts',(-37.7593608839214,-32.8596452685709,2.06420134993389));
#9250=CARTESIAN_POINT('Ctrl Pts',(-41.1877003796151,-33.4332762712177,1.9054166307082));
#9251=CARTESIAN_POINT('Ctrl Pts',(-43.5287246771368,-30.8638055949683,1.74663191148252));
#9252=CARTESIAN_POINT('Ctrl Pts',(-42.6392500792739,-27.5035231181503,1.58784719225684));
#9253=CARTESIAN_POINT('Ctrl Pts',(-39.333605094551,-26.4287480480142,1.42906247303115));
#9254=CARTESIAN_POINT('Ctrl Pts',(-36.6379947680772,-28.6233470921482,1.27027775380547));
#9255=CARTESIAN_POINT('Ctrl Pts',(-37.0203223217504,-32.078345102403,1.11149303457979));
#9256=CARTESIAN_POINT('Ctrl Pts',(-40.1303405334711,-33.6304608367794,0.952708315354102));
#9257=CARTESIAN_POINT('Ctrl Pts',(-43.1213437687621,-31.859332443099,0.793923596128418));
#9258=CARTESIAN_POINT('Ctrl Pts',(-43.2541899451756,-28.3852513068663,0.635138876902736));
#9259=CARTESIAN_POINT('Ctrl Pts',(-40.4091143639642,-26.3909743325875,0.47635415767705));
#9260=CARTESIAN_POINT('Ctrl Pts',(-37.1870296834247,-27.6976298827388,0.317569438451369));
#9261=CARTESIAN_POINT('Ctrl Pts',(-36.5451704756118,-31.1184197653857,0.158784719225683));
#9262=CARTESIAN_POINT('Ctrl Pts',(-38.2187620536724,-32.7052387009375,0.0529282397418946));
#9263=CARTESIAN_POINT('Ctrl Pts',(-39.2062007174671,-32.9692229537457,0.));
#9264=CARTESIAN_POINT('Ctrl Pts',(-39.2062007174671,-32.9692229537457,0.));
#9265=CARTESIAN_POINT('Ctrl Pts',(-39.1131466107856,-32.9351833458516,-1.6060879670377E-16));
#9266=CARTESIAN_POINT('Ctrl Pts',(-39.0221597277766,-32.8963742919489,-4.44513565583088E-16));
#9267=CARTESIAN_POINT('Ctrl Pts',(-38.9334478499662,-32.8531245205888,-6.10622663543836E-16));
#9268=CARTESIAN_POINT('Ctrl Pts',(-38.8427661867135,-32.8089144181874,-7.80420098298495E-16));
#9269=CARTESIAN_POINT('Ctrl Pts',(-38.7544610131422,-32.760063585673,-3.00700937848116E-15));
#9270=CARTESIAN_POINT('Ctrl Pts',(-38.6687831978432,-32.7068775858309,-3.05311331771918E-15));
#9271=CARTESIAN_POINT('Ctrl Pts',(-38.5858338035881,-32.655385300992,-3.09774907108449E-15));
#9272=CARTESIAN_POINT('Ctrl Pts',(-38.5053467696029,-32.5998286976775,-1.98203717691243E-15));
#9273=CARTESIAN_POINT('Ctrl Pts',(-38.4275834630713,-32.5404543773605,-2.16493489801906E-15));
#9274=CARTESIAN_POINT('Ctrl Pts',(-38.3595405698561,-32.4885018470831,-2.32497040398736E-15));
#9275=CARTESIAN_POINT('Ctrl Pts',(-38.2935833272372,-32.4336256602705,1.05568646747328E-15));
#9276=CARTESIAN_POINT('Ctrl Pts',(-38.2299120950925,-32.3759780448687,2.27595720048157E-15));
#9277=CARTESIAN_POINT('Ctrl Pts',(-38.2165695179232,-32.363897742176,2.53167011625481E-15));
#9278=CARTESIAN_POINT('Ctrl Pts',(-38.2033255561917,-32.3516938355638,-1.36442326856797E-15));
#9279=CARTESIAN_POINT('Ctrl Pts',(-38.1901992329768,-32.3393840298394,-1.38777878078145E-15));
#9280=CARTESIAN_POINT('Ctrl Pts',(-38.1177716356207,-32.2714617611321,-1.51664835125835E-15));
#9281=CARTESIAN_POINT('Ctrl Pts',(-38.0488097561366,-32.2002182797225,-1.51379216107608E-15));
#9282=CARTESIAN_POINT('Ctrl Pts',(-37.9835529381418,-32.125944757074,-1.16573417585641E-15));
#9283=CARTESIAN_POINT('Ctrl Pts',(-37.9186574569704,-32.0520824980997,-8.19603440089208E-16));
#9284=CARTESIAN_POINT('Ctrl Pts',(-37.8574256347879,-31.9752228624939,6.49623181554391E-16));
#9285=CARTESIAN_POINT('Ctrl Pts',(-37.8001364752534,-31.8956254663677,3.33066907387547E-16));
#9286=CARTESIAN_POINT('Ctrl Pts',(-37.7442813766686,-31.8180205504665,2.44346627378703E-17));
#9287=CARTESIAN_POINT('Ctrl Pts',(-37.6921737559928,-31.7378124817103,9.32925077816174E-16));
#9288=CARTESIAN_POINT('Ctrl Pts',(-37.6441190472323,-31.6552277434766,1.16573417585641E-15));
#9289=CARTESIAN_POINT('Ctrl Pts',(-37.6233914631522,-31.619606216479,1.26615243410233E-15));
#9290=CARTESIAN_POINT('Ctrl Pts',(-37.6034185407569,-31.5835423973841,-2.77132270277859E-15));
#9291=CARTESIAN_POINT('Ctrl Pts',(-37.584227773746,-31.5470541286155,-3.08086889333481E-15));
#9292=CARTESIAN_POINT('Ctrl Pts',(-37.5705624211823,-31.5210715789405,-3.30129040261011E-15));
#9293=CARTESIAN_POINT('Ctrl Pts',(-37.5572937042546,-31.4948738056765,1.83855327584014E-15));
#9294=CARTESIAN_POINT('Ctrl Pts',(-37.5444321465139,-31.4684672473934,1.80411241501588E-15));
#9295=CARTESIAN_POINT('Ctrl Pts',(-37.5388166481749,-31.4569378520303,1.78907515431618E-15));
#9296=CARTESIAN_POINT('Ctrl Pts',(-37.5332796940573,-31.4453704534221,7.2015229496451E-16));
#9297=CARTESIAN_POINT('Ctrl Pts',(-37.5278258543441,-31.4337738641374,6.38378239159465E-16));
#9298=CARTESIAN_POINT('Ctrl Pts',(-37.487598010987,-31.3482367376823,3.52079810388171E-17));
#9299=CARTESIAN_POINT('Ctrl Pts',(-37.4518262054158,-31.2609864756373,-4.26555916893969E-15));
#9300=CARTESIAN_POINT('Ctrl Pts',(-37.4207614166239,-31.1722603981052,-3.63598040564739E-15));
#9301=CARTESIAN_POINT('Ctrl Pts',(-37.3903833382621,-31.085495676991,-3.0203189526013E-15));
#9302=CARTESIAN_POINT('Ctrl Pts',(-37.3645062551562,-30.9973189926276,-6.38813711439151E-16));
#9303=CARTESIAN_POINT('Ctrl Pts',(-37.3434139855678,-30.9079434560133,-1.60982338570648E-15));
#9304=CARTESIAN_POINT('Ctrl Pts',(-37.3396853045659,-30.8921436927865,-1.7814779964148E-15));
#9305=CARTESIAN_POINT('Ctrl Pts',(-37.3361062849538,-30.8763064560273,-1.28296660226899E-15));
#9306=CARTESIAN_POINT('Ctrl Pts',(-37.3326786669098,-30.8604329174724,-1.2490009027033E-15));
#9307=CARTESIAN_POINT('Ctrl Pts',(-37.3125677659889,-30.7672979307153,-1.02302944293106E-15));
#9308=CARTESIAN_POINT('Ctrl Pts',(-37.2976648337907,-30.6729122002239,-7.87763452680115E-16));
#9309=CARTESIAN_POINT('Ctrl Pts',(-37.2878913789518,-30.5776846228188,-2.22044604925031E-16));
#9310=CARTESIAN_POINT('Ctrl Pts',(-37.2846134893309,-30.5457465320667,-3.23098621953069E-17));
#9311=CARTESIAN_POINT('Ctrl Pts',(-37.2819130028101,-30.513713867855,-1.58807512465196E-15));
#9312=CARTESIAN_POINT('Ctrl Pts',(-37.2797881830403,-30.4816025255615,-1.66533453693773E-15));
#9313=CARTESIAN_POINT('Ctrl Pts',(-37.2785995619339,-30.4636394871208,-1.70855334044072E-15));
#9314=CARTESIAN_POINT('Ctrl Pts',(-37.2775910929928,-30.4456518334769,1.44829596815902E-15));
#9315=CARTESIAN_POINT('Ctrl Pts',(-37.2767625516214,-30.4276423921194,1.77635683940025E-15));
#9316=CARTESIAN_POINT('Ctrl Pts',(-37.276188285258,-30.4151599540007,2.00373754728324E-15));
#9317=CARTESIAN_POINT('Ctrl Pts',(-37.2757005703862,-30.4026685786166,-6.72593298636936E-16));
#9318=CARTESIAN_POINT('Ctrl Pts',(-37.2752994571504,-30.3901786876117,-5.82867087928207E-16));
#9319=CARTESIAN_POINT('Ctrl Pts',(-37.2723066310671,-30.2969878670748,8.66070649168054E-17));
#9320=CARTESIAN_POINT('Ctrl Pts',(-37.2741233925594,-30.2037325944215,1.1534185885948E-15));
#9321=CARTESIAN_POINT('Ctrl Pts',(-37.280610638584,-30.1107879986708,1.01307850997046E-15));
#9322=CARTESIAN_POINT('Ctrl Pts',(-37.2871108431702,-30.0176577419689,8.72458095816411E-16));
#9323=CARTESIAN_POINT('Ctrl Pts',(-37.2983005933798,-29.9248384229594,-3.4945567965877E-15));
#9324=CARTESIAN_POINT('Ctrl Pts',(-37.314090996424,-29.8327194250238,-2.87270207621759E-15));
#9325=CARTESIAN_POINT('Ctrl Pts',(-37.3296582910756,-29.7419020101763,-2.25963376913325E-15));
#9326=CARTESIAN_POINT('Ctrl Pts',(-37.3496976162604,-29.6517644189367,7.72310224401951E-16));
#9327=CARTESIAN_POINT('Ctrl Pts',(-37.3741668412413,-29.5627049129401,1.0547118733939E-15));
#9328=CARTESIAN_POINT('Ctrl Pts',(-37.3836805051461,-29.5280784706137,1.1645099718931E-15));
#9329=CARTESIAN_POINT('Ctrl Pts',(-37.3938642491001,-29.4936153373462,-7.07244990223136E-16));
#9330=CARTESIAN_POINT('Ctrl Pts',(-37.4047171636237,-29.4593403829489,-6.10622663543836E-16));
#9331=CARTESIAN_POINT('Ctrl Pts',(-37.4105213799507,-29.4410098921402,-5.58948352016791E-16));
#9332=CARTESIAN_POINT('Ctrl Pts',(-37.4165170058423,-29.422733239581,1.26908615097469E-15));
#9333=CARTESIAN_POINT('Ctrl Pts',(-37.4227039978848,-29.4045143438212,1.13797860024079E-15));
#9334=CARTESIAN_POINT('Ctrl Pts',(-37.4281525928791,-29.3884698130449,1.02251830228993E-15));
#9335=CARTESIAN_POINT('Ctrl Pts',(-37.433750081042,-29.3724690012651,1.19736360869678E-15));
#9336=CARTESIAN_POINT('Ctrl Pts',(-37.4394903112345,-29.3565309947013,1.08246744900953E-15));
#9337=CARTESIAN_POINT('Ctrl Pts',(-37.4719157874641,-29.2665002057519,4.33440742784894E-16));
#9338=CARTESIAN_POINT('Ctrl Pts',(-37.5089323079084,-29.1783481505351,-1.87205846606356E-15));
#9339=CARTESIAN_POINT('Ctrl Pts',(-37.5504668382682,-29.0925193983103,-1.58206781009085E-15));
#9340=CARTESIAN_POINT('Ctrl Pts',(-37.581617736038,-29.0281478341417,-1.36457481811132E-15));
#9341=CARTESIAN_POINT('Ctrl Pts',(-37.6153111627318,-28.9650836648662,-1.04020469733639E-15));
#9342=CARTESIAN_POINT('Ctrl Pts',(-37.6515336753454,-28.9035316000466,-5.55111512312578E-17));
#9343=CARTESIAN_POINT('Ctrl Pts',(-37.6664654555227,-28.8781583767379,3.50402920200024E-16));
#9344=CARTESIAN_POINT('Ctrl Pts',(-37.6818271624147,-28.8530423027494,2.30518069273612E-15));
#9345=CARTESIAN_POINT('Ctrl Pts',(-37.6976185122319,-28.8281986233529,2.70616862252382E-15));
#9346=CARTESIAN_POINT('Ctrl Pts',(-37.7070511545528,-28.8133587556787,2.94569062415713E-15));
#9347=CARTESIAN_POINT('Ctrl Pts',(-37.7166324161044,-28.7986234989397,1.52399745346112E-15));
#9348=CARTESIAN_POINT('Ctrl Pts',(-37.7263602579883,-28.7839981748651,1.3392065234541E-15));
#9349=CARTESIAN_POINT('Ctrl Pts',(-37.7738889351269,-28.7125411842724,4.3634764116111E-16));
#9350=CARTESIAN_POINT('Ctrl Pts',(-37.8249264001993,-28.6436861696345,1.61280770038306E-15));
#9351=CARTESIAN_POINT('Ctrl Pts',(-37.8794382711486,-28.5777858428738,1.28022592527088E-15));
#9352=CARTESIAN_POINT('Ctrl Pts',(-37.9310243099595,-28.5154226042852,9.65494912375114E-16));
#9353=CARTESIAN_POINT('Ctrl Pts',(-37.9857222891604,-28.4557051705816,1.05564516917403E-15));
#9354=CARTESIAN_POINT('Ctrl Pts',(-38.0435268618259,-28.3989683289331,2.25470683790086E-15));
#9355=CARTESIAN_POINT('Ctrl Pts',(-38.0564928356052,-28.3862418547597,2.53840998574205E-15));
#9356=CARTESIAN_POINT('Ctrl Pts',(-38.0696151991774,-28.3736655038365,-1.14231766349927E-17));
#9357=CARTESIAN_POINT('Ctrl Pts',(-38.0828907223999,-28.3612406061267,5.55111512312578E-17));
#9358=CARTESIAN_POINT('Ctrl Pts',(-38.0865340033349,-28.364012796625,10.));
#9359=CARTESIAN_POINT('Ctrl Pts',(-38.0249212788374,-28.4219136285024,10.));
#9360=CARTESIAN_POINT('Ctrl Pts',(-37.9666797322405,-28.4829649756762,10.));
#9361=CARTESIAN_POINT('Ctrl Pts',(-37.9118062499715,-28.546782039445,10.));
#9362=CARTESIAN_POINT('Ctrl Pts',(-37.8554800838191,-28.6122885534946,10.));
#9363=CARTESIAN_POINT('Ctrl Pts',(-37.8027022343369,-28.6807095897459,10.));
#9364=CARTESIAN_POINT('Ctrl Pts',(-37.7534948834915,-28.7516775265204,10.));
#9365=CARTESIAN_POINT('Ctrl Pts',(-37.702593238571,-28.825089011926,10.));
#9366=CARTESIAN_POINT('Ctrl Pts',(-37.6555116194557,-28.9012263275327,10.));
#9367=CARTESIAN_POINT('Ctrl Pts',(-37.6123095085901,-28.9797265490615,10.));
#9368=CARTESIAN_POINT('Ctrl Pts',(-37.5934085850863,-29.0140703959804,10.));
#9369=CARTESIAN_POINT('Ctrl Pts',(-37.5752507177294,-29.0488670241427,10.));
#9370=CARTESIAN_POINT('Ctrl Pts',(-37.5578433328344,-29.084088131034,10.));
#9371=CARTESIAN_POINT('Ctrl Pts',(-37.5483351016093,-29.1033265422224,10.));
#9372=CARTESIAN_POINT('Ctrl Pts',(-37.5390508073497,-29.1226916181739,10.));
#9373=CARTESIAN_POINT('Ctrl Pts',(-37.5299918639726,-29.1421788751806,10.));
#9374=CARTESIAN_POINT('Ctrl Pts',(-37.5213418802068,-29.1607863937102,10.));
#9375=CARTESIAN_POINT('Ctrl Pts',(-37.5128948696392,-29.1795113098859,10.));
#9376=CARTESIAN_POINT('Ctrl Pts',(-37.5046661632847,-29.1983169400782,10.));
#9377=CARTESIAN_POINT('Ctrl Pts',(-37.4681053960581,-29.2818717831342,10.));
#9378=CARTESIAN_POINT('Ctrl Pts',(-37.4358048459705,-29.3671100877142,10.));
#9379=CARTESIAN_POINT('Ctrl Pts',(-37.4077887832518,-29.4536330059159,10.));
#9380=CARTESIAN_POINT('Ctrl Pts',(-37.3793104271871,-29.5415836397024,10.));
#9381=CARTESIAN_POINT('Ctrl Pts',(-37.3552586298795,-29.6308623874248,10.));
#9382=CARTESIAN_POINT('Ctrl Pts',(-37.3356979907178,-29.7210874579434,10.));
#9383=CARTESIAN_POINT('Ctrl Pts',(-37.3164756210823,-29.8097522322151,10.));
#9384=CARTESIAN_POINT('Ctrl Pts',(-37.3015901593891,-29.8993317913654,10.));
#9385=CARTESIAN_POINT('Ctrl Pts',(-37.2911456116882,-29.9894866561166,10.));
#9386=CARTESIAN_POINT('Ctrl Pts',(-37.2870154699214,-30.0251370627254,10.));
#9387=CARTESIAN_POINT('Ctrl Pts',(-37.2835802457749,-30.0608776102139,10.));
#9388=CARTESIAN_POINT('Ctrl Pts',(-37.2808483993985,-30.0966878419291,10.));
#9389=CARTESIAN_POINT('Ctrl Pts',(-37.279231497492,-30.1178828960977,10.));
#9390=CARTESIAN_POINT('Ctrl Pts',(-37.2778610197106,-30.13910236557,10.));
#9391=CARTESIAN_POINT('Ctrl Pts',(-37.276738922573,-30.1603420317173,10.));
#9392=CARTESIAN_POINT('Ctrl Pts',(-37.275992018335,-30.1744798421861,10.));
#9393=CARTESIAN_POINT('Ctrl Pts',(-37.2753552426062,-30.1886265975985,10.));
#9394=CARTESIAN_POINT('Ctrl Pts',(-37.2748295234487,-30.2027664976382,10.));
#9395=CARTESIAN_POINT('Ctrl Pts',(-37.2712907888299,-30.2979453646585,10.));
#9396=CARTESIAN_POINT('Ctrl Pts',(-37.2727707826484,-30.3929751968539,10.));
#9397=CARTESIAN_POINT('Ctrl Pts',(-37.2793281519079,-30.4874572708813,10.));
#9398=CARTESIAN_POINT('Ctrl Pts',(-37.2858630328702,-30.5816153215274,10.));
#9399=CARTESIAN_POINT('Ctrl Pts',(-37.2974401643112,-30.6752303180479,10.));
#9400=CARTESIAN_POINT('Ctrl Pts',(-37.3141655895868,-30.7679255281587,10.));
#9401=CARTESIAN_POINT('Ctrl Pts',(-37.3161024540939,-30.7786599674617,10.));
#9402=CARTESIAN_POINT('Ctrl Pts',(-37.318108416306,-30.7893820824334,10.));
#9403=CARTESIAN_POINT('Ctrl Pts',(-37.3201836861397,-30.8000912944808,10.));
#9404=CARTESIAN_POINT('Ctrl Pts',(-37.3377286165496,-30.8906300654228,10.));
#9405=CARTESIAN_POINT('Ctrl Pts',(-37.3602229262488,-30.9802469068505,10.));
#9406=CARTESIAN_POINT('Ctrl Pts',(-37.3873913235099,-31.0687038922713,10.));
#9407=CARTESIAN_POINT('Ctrl Pts',(-37.3981396071766,-31.1036989919992,10.));
#9408=CARTESIAN_POINT('Ctrl Pts',(-37.4096200259303,-31.1385125085135,10.));
#9409=CARTESIAN_POINT('Ctrl Pts',(-37.4218177279703,-31.1731293672529,10.));
#9410=CARTESIAN_POINT('Ctrl Pts',(-37.4277721424854,-31.1900278884227,10.));
#9411=CARTESIAN_POINT('Ctrl Pts',(-37.4338975028831,-31.2068795420036,10.));
#9412=CARTESIAN_POINT('Ctrl Pts',(-37.4401921825299,-31.2236825462617,10.));
#9413=CARTESIAN_POINT('Ctrl Pts',(-37.4454367253902,-31.2376823176491,10.));
#9414=CARTESIAN_POINT('Ctrl Pts',(-37.4507959097479,-31.251640508919,10.));
#9415=CARTESIAN_POINT('Ctrl Pts',(-37.4562665217367,-31.2655515407123,10.));
#9416=CARTESIAN_POINT('Ctrl Pts',(-37.4904911315776,-31.3525801284799,10.));
#9417=CARTESIAN_POINT('Ctrl Pts',(-37.5290941815582,-31.4378205888918,10.));
#9418=CARTESIAN_POINT('Ctrl Pts',(-37.5717431863619,-31.5210410503347,10.));
#9419=CARTESIAN_POINT('Ctrl Pts',(-37.6159724064538,-31.6073449658009,10.));
#9420=CARTESIAN_POINT('Ctrl Pts',(-37.6645530837038,-31.6914771466329,10.));
#9421=CARTESIAN_POINT('Ctrl Pts',(-37.717170350465,-31.7731754529168,10.));
#9422=CARTESIAN_POINT('Ctrl Pts',(-37.7703652467546,-31.8557706388191,10.));
#9423=CARTESIAN_POINT('Ctrl Pts',(-37.8276862641756,-31.9358790367524,10.));
#9424=CARTESIAN_POINT('Ctrl Pts',(-37.8888596681732,-32.0132144212221,10.));
#9425=CARTESIAN_POINT('Ctrl Pts',(-37.9126768228721,-32.0433240553972,10.));
#9426=CARTESIAN_POINT('Ctrl Pts',(-37.9370784537989,-32.0730131141866,10.));
#9427=CARTESIAN_POINT('Ctrl Pts',(-37.9620502718248,-32.1022636654044,10.));
#9428=CARTESIAN_POINT('Ctrl Pts',(-37.9820385514047,-32.1256767863474,10.));
#9429=CARTESIAN_POINT('Ctrl Pts',(-38.0023921666863,-32.1488089475494,10.));
#9430=CARTESIAN_POINT('Ctrl Pts',(-38.0231042262141,-32.17165061074,10.));
#9431=CARTESIAN_POINT('Ctrl Pts',(-38.0346509963009,-32.1843846139862,10.));
#9432=CARTESIAN_POINT('Ctrl Pts',(-38.0463040959221,-32.1970226665823,10.));
#9433=CARTESIAN_POINT('Ctrl Pts',(-38.0580572806936,-32.2095583549418,10.));
#9434=CARTESIAN_POINT('Ctrl Pts',(-38.1271126580838,-32.2832113015552,10.));
#9435=CARTESIAN_POINT('Ctrl Pts',(-38.1996686238852,-32.3533868119705,10.));
#9436=CARTESIAN_POINT('Ctrl Pts',(-38.2754132400136,-32.4197960351437,10.));
#9437=CARTESIAN_POINT('Ctrl Pts',(-38.3396640840132,-32.476128073727,10.));
#9438=CARTESIAN_POINT('Ctrl Pts',(-38.4062103469001,-32.5297501453147,10.));
#9439=CARTESIAN_POINT('Ctrl Pts',(-38.4748864946038,-32.5804710235722,10.));
#9440=CARTESIAN_POINT('Ctrl Pts',(-38.4975765316306,-32.5972287865536,10.));
#9441=CARTESIAN_POINT('Ctrl Pts',(-38.5204992313683,-32.6136697219234,10.));
#9442=CARTESIAN_POINT('Ctrl Pts',(-38.5436490948133,-32.629786492381,10.));
#9443=CARTESIAN_POINT('Ctrl Pts',(-38.5602427937514,-32.6413389076885,10.));
#9444=CARTESIAN_POINT('Ctrl Pts',(-38.5769541763244,-32.652725292037,10.));
#9445=CARTESIAN_POINT('Ctrl Pts',(-38.5937666592579,-32.6639334564857,10.));
#9446=CARTESIAN_POINT('Ctrl Pts',(-38.6801204794835,-32.721501860967,10.));
#9447=CARTESIAN_POINT('Ctrl Pts',(-38.7692236934361,-32.774432012051,10.));
#9448=CARTESIAN_POINT('Ctrl Pts',(-38.860767757559,-32.822402446742,10.));
#9449=CARTESIAN_POINT('Ctrl Pts',(-38.9523118216819,-32.8703728814329,10.));
#9450=CARTESIAN_POINT('Ctrl Pts',(-39.0462973813034,-32.9133845104196,10.));
#9451=CARTESIAN_POINT('Ctrl Pts',(-39.1424539364134,-32.951075124157,10.));
#9452=CARTESIAN_POINT('Ctrl Pts',(-39.1630219002104,-32.9591371764835,10.));
#9453=CARTESIAN_POINT('Ctrl Pts',(-39.1836893128189,-32.9669555963369,10.));
#9454=CARTESIAN_POINT('Ctrl Pts',(-39.2044522699742,-32.9745315604842,10.));
#9455=CARTESIAN_POINT('Ctrl Pts',(-42.51946795121,-30.0019779683886,8.38741669750802));
#9456=CARTESIAN_POINT('Ctrl Pts',(-42.5205894505478,-30.1321096272865,8.3956620675864));
#9457=CARTESIAN_POINT('Ctrl Pts',(-42.5113779533637,-30.2620820270818,8.40390743766478));
#9458=CARTESIAN_POINT('Ctrl Pts',(-42.4912804519573,-30.3903486209662,8.41215280774316));
#9459=CARTESIAN_POINT('Ctrl Pts',(-42.3622716430691,-31.213710697799,8.46508104748505));
#9460=CARTESIAN_POINT('Ctrl Pts',(-41.7847001994946,-31.9667842851201,8.51800928722694));
#9461=CARTESIAN_POINT('Ctrl Pts',(-41.0229436930189,-32.3048687922893,8.57093752696884));
#9462=CARTESIAN_POINT('Ctrl Pts',(-40.2611871865431,-32.6429532994586,8.62386576671073));
#9463=CARTESIAN_POINT('Ctrl Pts',(-39.3152456171661,-32.566048726476,8.67679400645262));
#9464=CARTESIAN_POINT('Ctrl Pts',(-38.6181178943748,-32.1093322946775,8.72972224619452));
#9465=CARTESIAN_POINT('Ctrl Pts',(-37.9209901715836,-31.652615862879,8.78265048593641));
#9466=CARTESIAN_POINT('Ctrl Pts',(-37.472676295378,-30.8160875722647,8.83557872567831));
#9467=CARTESIAN_POINT('Ctrl Pts',(-37.4783843069573,-29.9827116901432,8.8885069654202));
#9468=CARTESIAN_POINT('Ctrl Pts',(-37.4840923185365,-29.1493358080216,8.9414352051621));
#9469=CARTESIAN_POINT('Ctrl Pts',(-37.9438222179007,-28.3191123343929,8.994363444904));
#9470=CARTESIAN_POINT('Ctrl Pts',(-38.6471442946355,-27.8719686461583,9.04729168464589));
#9471=CARTESIAN_POINT('Ctrl Pts',(-39.3504663713704,-27.4248249579237,9.10021992438779));
#9472=CARTESIAN_POINT('Ctrl Pts',(-40.297380625476,-27.3607610550832,9.15314816412968));
#9473=CARTESIAN_POINT('Ctrl Pts',(-41.0544291986404,-27.7093025098685,9.20607640387157));
#9474=CARTESIAN_POINT('Ctrl Pts',(-41.8114777718049,-28.0578439646537,9.25900464361346));
#9475=CARTESIAN_POINT('Ctrl Pts',(-42.3786606640282,-28.8189907770648,9.31193288335536));
#9476=CARTESIAN_POINT('Ctrl Pts',(-42.4963858324552,-29.6439329582262,9.36486112309726));
#9477=CARTESIAN_POINT('Ctrl Pts',(-42.5131088446533,-29.7611170603394,9.37237964790084));
#9478=CARTESIAN_POINT('Ctrl Pts',(-42.5207624429925,-29.8795884617265,9.37989817270443));
#9479=CARTESIAN_POINT('Ctrl Pts',(-42.5197817068771,-29.9981833838556,9.38741669750801));
#9480=CARTESIAN_POINT('Ctrl Pts',(-40.7937992825329,-32.9692229537457,10.));
#9481=CARTESIAN_POINT('Ctrl Pts',(-41.7812379463276,-32.7052387009375,9.94707176025811));
#9482=CARTESIAN_POINT('Ctrl Pts',(-43.4548293913714,-31.1184189156626,9.84121528077431));
#9483=CARTESIAN_POINT('Ctrl Pts',(-42.8129704324572,-27.6976302329706,9.68243056154864));
#9484=CARTESIAN_POINT('Ctrl Pts',(-39.5908856218057,-26.3909740388041,9.52364584232295));
#9485=CARTESIAN_POINT('Ctrl Pts',(-36.745809981275,-28.3852514028181,9.36486112309727));
#9486=CARTESIAN_POINT('Ctrl Pts',(-36.8786561820279,-31.8593324073604,9.20607640387158));
#9487=CARTESIAN_POINT('Ctrl Pts',(-39.869659454766,-33.6304609478428,9.0472916846459));
#9488=CARTESIAN_POINT('Ctrl Pts',(-42.9796777427015,-32.0783451207568,8.88850696542022));
#9489=CARTESIAN_POINT('Ctrl Pts',(-43.3620052935445,-28.6233470774409,8.72972224619453));
#9490=CARTESIAN_POINT('Ctrl Pts',(-40.6663949208769,-26.4287479717036,8.57093752696886));
#9491=CARTESIAN_POINT('Ctrl Pts',(-37.3607498677919,-27.5035230729969,8.41215280774315));
#9492=CARTESIAN_POINT('Ctrl Pts',(-36.4712752548112,-30.8638056099088,8.25336808851749));
#9493=CARTESIAN_POINT('Ctrl Pts',(-38.8122995967417,-33.4332763392514,8.0945833692918));
#9494=CARTESIAN_POINT('Ctrl Pts',(-42.2406391600676,-32.8596453238364,7.93579865006611));
#9495=CARTESIAN_POINT('Ctrl Pts',(-43.6177130282472,-29.6680532348257,7.77701393084043));
#9496=CARTESIAN_POINT('Ctrl Pts',(-41.6828291578641,-26.7803544372571,7.61822921161475));
#9497=CARTESIAN_POINT('Ctrl Pts',(-38.2073436047123,-26.8401872096979,7.45944449238906));
#9498=CARTESIAN_POINT('Ctrl Pts',(-36.3730050616526,-29.7927767730296,7.30065977316338));
#9499=CARTESIAN_POINT('Ctrl Pts',(-37.8591206231434,-32.9350755877781,7.1418750539377));
#9500=CARTESIAN_POINT('Ctrl Pts',(-41.3051758117063,-33.390361281965,6.98309033471201));
#9501=CARTESIAN_POINT('Ctrl Pts',(-43.5563641435752,-30.7418271809609,6.82430561548632));
#9502=CARTESIAN_POINT('Ctrl Pts',(-42.5517598309746,-27.4141625739817,6.66552089626065));
#9503=CARTESIAN_POINT('Ctrl Pts',(-39.2110615557591,-26.4537894026696,6.50673617703496));
#9504=CARTESIAN_POINT('Ctrl Pts',(-36.592623388795,-28.7399134586708,6.34795145780928));
#9505=CARTESIAN_POINT('Ctrl Pts',(-37.0935822247194,-32.1796259246658,6.18916673858359));
#9506=CARTESIAN_POINT('Ctrl Pts',(-40.2553185210464,-33.623926863772,6.03038201935791));
#9507=CARTESIAN_POINT('Ctrl Pts',(-43.1833149296159,-31.7505826226676,5.87159730013223));
#9508=CARTESIAN_POINT('Ctrl Pts',(-43.1970391055899,-28.2746089090863,5.71281258090654));
#9509=CARTESIAN_POINT('Ctrl Pts',(-40.2839267930322,-26.378202236992,5.55402786168086));
#9510=CARTESIAN_POINT('Ctrl Pts',(-37.1108841916168,-27.7974915878749,5.39524314245518));
#9511=CARTESIAN_POINT('Ctrl Pts',(-36.5827793869729,-31.2331410063646,5.23645842322949));
#9512=CARTESIAN_POINT('Ctrl Pts',(-39.1830836038332,-33.5398702040376,5.07767370400381));
#9513=CARTESIAN_POINT('Ctrl Pts',(-42.5312612865998,-32.605906705675,4.91888898477813));
#9514=CARTESIAN_POINT('Ctrl Pts',(-43.5621110758558,-29.2862786657343,4.76010426555244));
#9515=CARTESIAN_POINT('Ctrl Pts',(-41.3319070183432,-26.6200507172078,4.60131954632676));
#9516=CARTESIAN_POINT('Ctrl Pts',(-37.8823640875572,-27.0481105030832,4.44253482710108));
#9517=CARTESIAN_POINT('Ctrl Pts',(-36.3714818529893,-30.1785763605433,4.28375010787539));
#9518=CARTESIAN_POINT('Ctrl Pts',(-38.1824480418478,-33.1455585099229,4.12496538864971));
#9519=CARTESIAN_POINT('Ctrl Pts',(-41.6573530239065,-33.2328338054134,3.96618066942403));
#9520=CARTESIAN_POINT('Ctrl Pts',(-43.6149786907205,-30.3605031560721,3.80739595019834));
#9521=CARTESIAN_POINT('Ctrl Pts',(-42.2631510826477,-27.1581378220842,3.64861123097266));
#9522=CARTESIAN_POINT('Ctrl Pts',(-38.8394460438999,-26.5574503676893,3.48982651174697));
#9523=CARTESIAN_POINT('Ctrl Pts',(-36.4782089804049,-29.1083602316377,3.33104179252129));
#9524=CARTESIAN_POINT('Ctrl Pts',(-37.341113418528,-32.4755515781919,3.17225707329561));
#9525=CARTESIAN_POINT('Ctrl Pts',(-40.6381845987477,-33.5764163413526,3.01347235406993));
#9526=CARTESIAN_POINT('Ctrl Pts',(-43.3510083223003,-31.4031310387823,2.85468763484424));
#9527=CARTESIAN_POINT('Ctrl Pts',(-42.9960392803275,-27.945302418251,2.69590291561856));
#9528=CARTESIAN_POINT('Ctrl Pts',(-39.898245774117,-26.3685155528715,2.53711819639287));
#9529=CARTESIAN_POINT('Ctrl Pts',(-36.8936065712748,-28.1162925878559,2.37833347716719));
#9530=CARTESIAN_POINT('Ctrl Pts',(-36.7328192563745,-31.5885728846373,2.2195487579415));
#9531=CARTESIAN_POINT('Ctrl Pts',(-39.5630819030797,-33.6065404615547,2.06076403871582));
#9532=CARTESIAN_POINT('Ctrl Pts',(-42.7933359259129,-32.3227807935024,1.90197931949014));
#9533=CARTESIAN_POINT('Ctrl Pts',(-43.4663369005618,-28.912551741198,1.74319460026445));
#9534=CARTESIAN_POINT('Ctrl Pts',(-40.9659640066834,-26.4978674771854,1.58440988103877));
#9535=CARTESIAN_POINT('Ctrl Pts',(-37.5812664167199,-27.2893199539358,1.42562516181309));
#9536=CARTESIAN_POINT('Ctrl Pts',(-36.410880674872,-30.5623706761659,1.26684044258741));
#9537=CARTESIAN_POINT('Ctrl Pts',(-38.5262719729362,-33.320549494049,1.10805572336172));
#9538=CARTESIAN_POINT('Ctrl Pts',(-41.9908417541182,-33.0388816977749,0.949271004136036));
#9539=CARTESIAN_POINT('Ctrl Pts',(-43.6328191716239,-29.9750448881763,0.790486284910355));
#9540=CARTESIAN_POINT('Ctrl Pts',(-41.9490298715236,-26.9342997681684,0.631701565684669));
#9541=CARTESIAN_POINT('Ctrl Pts',(-38.4808975311013,-26.6996618476225,0.472916846458986));
#9542=CARTESIAN_POINT('Ctrl Pts',(-36.4035550403569,-29.4874091667537,0.314132127233303));
#9543=CARTESIAN_POINT('Ctrl Pts',(-37.6185459416804,-32.7424659580649,0.155347408007618));
#9544=CARTESIAN_POINT('Ctrl Pts',(-41.0140166119162,-33.4907706181827,-0.00343731121806399));
#9545=CARTESIAN_POINT('Ctrl Pts',(-43.4806505248308,-31.0352675588419,-0.162222030443749));
#9546=CARTESIAN_POINT('Ctrl Pts',(-43.0002811455947,-28.7795746242083,-0.268078509927538));
#9547=CARTESIAN_POINT('Ctrl Pts',(-42.3360626576962,-28.0026984430693,-0.321006749669432));
#9548=CARTESIAN_POINT('Ctrl Pts',(-40.745932854347,-32.7901775698422,10.1070022498898));
#9549=CARTESIAN_POINT('Ctrl Pts',(-41.673828554412,-32.5421116777044,10.0540740101479));
#9550=CARTESIAN_POINT('Ctrl Pts',(-43.2465017365151,-31.0509777880547,9.94821753066413));
#9551=CARTESIAN_POINT('Ctrl Pts',(-42.6433471408303,-27.836464091272,9.78943281143844));
#9552=CARTESIAN_POINT('Ctrl Pts',(-39.6155553896356,-26.6085998112053,9.63064809221276));
#9553=CARTESIAN_POINT('Ctrl Pts',(-36.9420389981841,-28.482621417463,9.47186337298707));
#9554=CARTESIAN_POINT('Ctrl Pts',(-37.0668745175621,-31.7472138868363,9.31307865376139));
#9555=CARTESIAN_POINT('Ctrl Pts',(-39.877519044067,-33.4115426367967,9.1542939345357));
#9556=CARTESIAN_POINT('Ctrl Pts',(-42.8000019306586,-31.9530200421666,8.99550921531003));
#9557=CARTESIAN_POINT('Ctrl Pts',(-43.1592749705456,-28.7063598234897,8.83672449608434));
#9558=CARTESIAN_POINT('Ctrl Pts',(-40.6262110288963,-26.6440959601784,8.67793977685866));
#9559=CARTESIAN_POINT('Ctrl Pts',(-37.5198977527772,-27.6540616740938,8.51915505763297));
#9560=CARTESIAN_POINT('Ctrl Pts',(-36.6840588303576,-30.8117177709512,8.3603703384073));
#9561=CARTESIAN_POINT('Ctrl Pts',(-38.8839184269799,-33.2262483424373,8.2015856191816));
#9562=CARTESIAN_POINT('Ctrl Pts',(-42.1055276831414,-32.6872075167703,8.04280089995592));
#9563=CARTESIAN_POINT('Ctrl Pts',(-43.3995634220756,-29.6880697633694,7.88401618073025));
#9564=CARTESIAN_POINT('Ctrl Pts',(-41.5813538569833,-26.9745004090466,7.72523146150455));
#9565=CARTESIAN_POINT('Ctrl Pts',(-38.315441533868,-27.0307252403262,7.56644674227887));
#9566=CARTESIAN_POINT('Ctrl Pts',(-36.5917143708789,-29.8052724201415,7.40766202305319));
#9567=CARTESIAN_POINT('Ctrl Pts',(-37.9882165434875,-32.7580893043005,7.24887730382751));
#9568=CARTESIAN_POINT('Ctrl Pts',(-41.226473165287,-33.1859210810244,7.09009258460182));
#9569=CARTESIAN_POINT('Ctrl Pts',(-43.3419139007655,-30.6970946922006,6.93130786537613));
#9570=CARTESIAN_POINT('Ctrl Pts',(-42.397887647685,-27.5700896504815,6.77252314615046));
#9571=CARTESIAN_POINT('Ctrl Pts',(-39.2586348733664,-26.6676273824012,6.61373842692477));
#9572=CARTESIAN_POINT('Ctrl Pts',(-36.7980896211934,-28.8158972032594,6.45495370769909));
#9573=CARTESIAN_POINT('Ctrl Pts',(-37.2688404301373,-32.0481935713103,6.2961689884734));
#9574=CARTESIAN_POINT('Ctrl Pts',(-40.2399227076196,-33.4054025607237,6.13738426924772));
#9575=CARTESIAN_POINT('Ctrl Pts',(-42.9913597101737,-31.6450217595687,5.97859955002204));
#9576=CARTESIAN_POINT('Ctrl Pts',(-43.004256312606,-28.3786507123017,5.81981483079635));
#9577=CARTESIAN_POINT('Ctrl Pts',(-40.2668058888593,-26.5965981543753,5.66103011157067));
#9578=CARTESIAN_POINT('Ctrl Pts',(-37.2850990812065,-27.9303037647787,5.50224539234499));
#9579=CARTESIAN_POINT('Ctrl Pts',(-36.7888392167916,-31.1587820887854,5.3434606731193));
#9580=CARTESIAN_POINT('Ctrl Pts',(-39.2323440036238,-33.326414552669,5.18467595389362));
#9581=CARTESIAN_POINT('Ctrl Pts',(-42.378625174095,-32.448769443232,5.02589123466794));
#9582=CARTESIAN_POINT('Ctrl Pts',(-43.3473142906298,-29.3293163602033,4.86710651544225));
#9583=CARTESIAN_POINT('Ctrl Pts',(-41.2515924690022,-26.8238630702507,4.70832179621657));
#9584=CARTESIAN_POINT('Ctrl Pts',(-38.0100584172918,-27.2261106723024,4.54953707699089));
#9585=CARTESIAN_POINT('Ctrl Pts',(-36.590283012334,-30.1678081314383,4.39075235776521));
#9586=CARTESIAN_POINT('Ctrl Pts',(-38.2920471838393,-32.9558800183533,4.23196763853952));
#9587=CARTESIAN_POINT('Ctrl Pts',(-41.5574139445407,-33.0378925770842,4.07318291931383));
#9588=CARTESIAN_POINT('Ctrl Pts',(-43.3969939662434,-30.3387646652336,3.91439820008815));
#9589=CARTESIAN_POINT('Ctrl Pts',(-42.1266821273902,-27.329503298026,3.75561348086246));
#9590=CARTESIAN_POINT('Ctrl Pts',(-38.9094279320396,-26.7650375479468,3.59682876163679));
#9591=CARTESIAN_POINT('Ctrl Pts',(-36.6905744494028,-29.1621264819722,3.4380440424111));
#9592=CARTESIAN_POINT('Ctrl Pts',(-37.5014453896032,-32.3262747843657,3.27925932318542));
#9593=CARTESIAN_POINT('Ctrl Pts',(-40.5997018009706,-33.360756942644,3.12047460395974));
#9594=CARTESIAN_POINT('Ctrl Pts',(-43.1489411212593,-31.3185216512694,2.96168988473405));
#9595=CARTESIAN_POINT('Ctrl Pts',(-42.815376860734,-28.0692015403651,2.80290516550837));
#9596=CARTESIAN_POINT('Ctrl Pts',(-39.9043815964251,-26.5874955813519,2.64412044628268));
#9597=CARTESIAN_POINT('Ctrl Pts',(-37.0809233920948,-28.2298809313462,2.485335727057));
#9598=CARTESIAN_POINT('Ctrl Pts',(-36.9298316194194,-31.4927812763885,2.32655100783131));
#9599=CARTESIAN_POINT('Ctrl Pts',(-39.5894282467582,-33.3890645658197,2.16776628860563));
#9600=CARTESIAN_POINT('Ctrl Pts',(-42.624896603229,-32.1827161417821,2.00898156937995));
#9601=CARTESIAN_POINT('Ctrl Pts',(-43.2573153380963,-28.9781253252655,1.85019685015427));
#9602=CARTESIAN_POINT('Ctrl Pts',(-40.9077159737442,-26.7090475306191,1.69141213092858));
#9603=CARTESIAN_POINT('Ctrl Pts',(-37.7271170617287,-27.4527750925521,1.5326274117029));
#9604=CARTESIAN_POINT('Ctrl Pts',(-36.6273060688062,-30.5284594895764,1.37384269247722));
#9605=CARTESIAN_POINT('Ctrl Pts',(-38.6151383883202,-33.1203189730695,1.21505797325153));
#9606=CARTESIAN_POINT('Ctrl Pts',(-41.8707931650731,-32.8556358625206,1.05627325402585));
#9607=CARTESIAN_POINT('Ctrl Pts',(-43.4137586586991,-29.9765496918393,0.897488534800165));
#9608=CARTESIAN_POINT('Ctrl Pts',(-41.8315025564575,-27.1191627722244,0.73870381557448));
#9609=CARTESIAN_POINT('Ctrl Pts',(-38.5725000442738,-26.8986736162599,0.579919096348797));
#9610=CARTESIAN_POINT('Ctrl Pts',(-36.6204221731113,-29.5183186080297,0.421134377123114));
#9611=CARTESIAN_POINT('Ctrl Pts',(-37.7621486157681,-32.5770941156828,0.262349657897428));
#9612=CARTESIAN_POINT('Ctrl Pts',(-40.9528709868172,-33.2802756923425,0.103564938671747));
#9613=CARTESIAN_POINT('Ctrl Pts',(-43.2707658448453,-30.97284049277,-0.0552197805539385));
#9614=CARTESIAN_POINT('Ctrl Pts',(-42.8193629397544,-28.8531667839546,-0.161076260037727));
#9615=CARTESIAN_POINT('Ctrl Pts',(-42.1951971040191,-28.1231365609212,-0.214004499779622));
#9616=CARTESIAN_POINT('Ctrl Pts',(-40.698066426161,-32.6111321859386,10.2140044997796));
#9617=CARTESIAN_POINT('Ctrl Pts',(-41.5664191624963,-32.3789846544712,10.1610762600377));
#9618=CARTESIAN_POINT('Ctrl Pts',(-43.0381740816587,-30.9835366604468,10.0552197805539));
#9619=CARTESIAN_POINT('Ctrl Pts',(-42.4737238492034,-27.9752979495734,9.89643506132826));
#9620=CARTESIAN_POINT('Ctrl Pts',(-39.6402251574656,-26.8262255836064,9.73765034210257));
#9621=CARTESIAN_POINT('Ctrl Pts',(-37.1382680150933,-28.5799914321079,9.57886562287689));
#9622=CARTESIAN_POINT('Ctrl Pts',(-37.2550928530962,-31.6350953663122,9.4200809036512));
#9623=CARTESIAN_POINT('Ctrl Pts',(-39.8853786333681,-33.1926243257506,9.26129618442552));
#9624=CARTESIAN_POINT('Ctrl Pts',(-42.6203261186156,-31.8276949635764,9.10251146519983));
#9625=CARTESIAN_POINT('Ctrl Pts',(-42.9565446475468,-28.7893725695385,8.94372674597416));
#9626=CARTESIAN_POINT('Ctrl Pts',(-40.5860271369156,-26.8594439486533,8.78494202674846));
#9627=CARTESIAN_POINT('Ctrl Pts',(-37.6790456377626,-27.8046002751907,8.62615730752279));
#9628=CARTESIAN_POINT('Ctrl Pts',(-36.8968424059039,-30.7596299319935,8.4673725882971));
#9629=CARTESIAN_POINT('Ctrl Pts',(-38.9555372572181,-33.0192203456233,8.30858786907142));
#9630=CARTESIAN_POINT('Ctrl Pts',(-41.9704162062153,-32.5147697097042,8.14980314984574));
#9631=CARTESIAN_POINT('Ctrl Pts',(-43.181413815904,-29.7080862919131,7.99101843062005));
#9632=CARTESIAN_POINT('Ctrl Pts',(-41.4798785561023,-27.1686463808361,7.83223371139437));
#9633=CARTESIAN_POINT('Ctrl Pts',(-38.4235394630237,-27.2212632709545,7.67344899216868));
#9634=CARTESIAN_POINT('Ctrl Pts',(-36.8104236801052,-29.8177680672534,7.51466427294301));
#9635=CARTESIAN_POINT('Ctrl Pts',(-38.1173124638315,-32.5811030208231,7.35587955371732));
#9636=CARTESIAN_POINT('Ctrl Pts',(-41.1477705188678,-32.9814808800838,7.19709483449163));
#9637=CARTESIAN_POINT('Ctrl Pts',(-43.1274636579556,-30.6523622034403,7.03831011526595));
#9638=CARTESIAN_POINT('Ctrl Pts',(-42.2440154643954,-27.7260167269812,6.87952539604026));
#9639=CARTESIAN_POINT('Ctrl Pts',(-39.3062081909736,-26.8814653621329,6.72074067681458));
#9640=CARTESIAN_POINT('Ctrl Pts',(-37.0035558535919,-28.891880947848,6.5619559575889));
#9641=CARTESIAN_POINT('Ctrl Pts',(-37.4440986355553,-31.9167612179548,6.40317123836321));
#9642=CARTESIAN_POINT('Ctrl Pts',(-40.2245268941928,-33.1868782576754,6.24438651913754));
#9643=CARTESIAN_POINT('Ctrl Pts',(-42.7994044907315,-31.5394608964698,6.08560179991185));
#9644=CARTESIAN_POINT('Ctrl Pts',(-42.8114735196222,-28.4826925155172,5.92681708068617));
#9645=CARTESIAN_POINT('Ctrl Pts',(-40.2496849846864,-26.8149940717586,5.76803236146048));
#9646=CARTESIAN_POINT('Ctrl Pts',(-37.4593139707961,-28.0631159416825,5.6092476422348));
#9647=CARTESIAN_POINT('Ctrl Pts',(-36.9948990466102,-31.0844231712062,5.45046292300912));
#9648=CARTESIAN_POINT('Ctrl Pts',(-39.2816044034143,-33.1129589013003,5.29167820378343));
#9649=CARTESIAN_POINT('Ctrl Pts',(-42.2259890615903,-32.2916321807891,5.13289348455775));
#9650=CARTESIAN_POINT('Ctrl Pts',(-43.1325175054039,-29.3723540546723,4.97410876533206));
#9651=CARTESIAN_POINT('Ctrl Pts',(-41.1712779196612,-27.0276754232936,4.81532404610638));
#9652=CARTESIAN_POINT('Ctrl Pts',(-38.1377527470264,-27.4041108415216,4.6565393268807));
#9653=CARTESIAN_POINT('Ctrl Pts',(-36.8090841716787,-30.1570399023334,4.49775460765501));
#9654=CARTESIAN_POINT('Ctrl Pts',(-38.4016463258308,-32.7662015267838,4.33896988842933));
#9655=CARTESIAN_POINT('Ctrl Pts',(-41.457474865175,-32.8429513487549,4.18018516920364));
#9656=CARTESIAN_POINT('Ctrl Pts',(-43.1790092417664,-30.3170261743952,4.02140044997796));
#9657=CARTESIAN_POINT('Ctrl Pts',(-41.9902131721327,-27.5008687739677,3.86261573075228));
#9658=CARTESIAN_POINT('Ctrl Pts',(-38.9794098201792,-26.9726247282044,3.70383101152659));
#9659=CARTESIAN_POINT('Ctrl Pts',(-36.9029399184007,-29.2158927323067,3.54504629230091));
#9660=CARTESIAN_POINT('Ctrl Pts',(-37.6617773606783,-32.1769979905394,3.38626157307523));
#9661=CARTESIAN_POINT('Ctrl Pts',(-40.5612190031936,-33.1450975439355,3.22747685384954));
#9662=CARTESIAN_POINT('Ctrl Pts',(-42.9468739202182,-31.2339122637565,3.06869213462387));
#9663=CARTESIAN_POINT('Ctrl Pts',(-42.6347144411405,-28.1931006624791,2.90990741539817));
#9664=CARTESIAN_POINT('Ctrl Pts',(-39.9105174187331,-26.8064756098323,2.7511226961725));
#9665=CARTESIAN_POINT('Ctrl Pts',(-37.2682402129149,-28.3434692748364,2.59233797694681));
#9666=CARTESIAN_POINT('Ctrl Pts',(-37.1268439824643,-31.3969896681396,2.43355325772113));
#9667=CARTESIAN_POINT('Ctrl Pts',(-39.6157745904367,-33.1715886700848,2.27476853849544));
#9668=CARTESIAN_POINT('Ctrl Pts',(-42.456457280545,-32.0426514900617,2.11598381926976));
#9669=CARTESIAN_POINT('Ctrl Pts',(-43.048293775631,-29.0436989093329,1.95719910004408));
#9670=CARTESIAN_POINT('Ctrl Pts',(-40.8494679408049,-26.9202275840527,1.79841438081839));
#9671=CARTESIAN_POINT('Ctrl Pts',(-37.8729677067375,-27.6162302311684,1.63962966159271));
#9672=CARTESIAN_POINT('Ctrl Pts',(-36.8437314627405,-30.494548302987,1.48084494236703));
#9673=CARTESIAN_POINT('Ctrl Pts',(-38.7040048037041,-32.92008845209,1.32206022314134));
#9674=CARTESIAN_POINT('Ctrl Pts',(-41.7507445760281,-32.6723900272662,1.16327550391566));
#9675=CARTESIAN_POINT('Ctrl Pts',(-43.1946981457743,-29.9780544955022,1.00449078468998));
#9676=CARTESIAN_POINT('Ctrl Pts',(-41.7139752413914,-27.3040257762804,0.845706065464291));
#9677=CARTESIAN_POINT('Ctrl Pts',(-38.6641025574464,-27.0976853848974,0.686921346238608));
#9678=CARTESIAN_POINT('Ctrl Pts',(-36.8372893058656,-29.5492280493056,0.528136627012925));
#9679=CARTESIAN_POINT('Ctrl Pts',(-37.9057512898559,-32.4117222733007,0.369351907787239));
#9680=CARTESIAN_POINT('Ctrl Pts',(-40.8917253617181,-33.0697807665023,0.210567188561557));
#9681=CARTESIAN_POINT('Ctrl Pts',(-43.0608811648599,-30.9104134266981,0.0517824693358723));
#9682=CARTESIAN_POINT('Ctrl Pts',(-42.6384447339141,-28.9267589437008,-0.0540740101479163));
#9683=CARTESIAN_POINT('Ctrl Pts',(-42.0543315503421,-28.2435746787731,-0.107002249889811));
#9684=CARTESIAN_POINT('Ctrl Pts',(-40.6501999979751,-32.4320868020351,10.3210067496694));
#9685=CARTESIAN_POINT('Ctrl Pts',(-41.4590097705807,-32.2158576312381,10.2680785099275));
#9686=CARTESIAN_POINT('Ctrl Pts',(-42.8298464268025,-30.916095532839,10.1622220304438));
#9687=CARTESIAN_POINT('Ctrl Pts',(-42.3041005575764,-28.1141318078749,10.0034373112181));
#9688=CARTESIAN_POINT('Ctrl Pts',(-39.6648949252955,-27.0438513560076,9.84465259199239));
#9689=CARTESIAN_POINT('Ctrl Pts',(-37.3344970320025,-28.6773614467528,9.68586787276669));
#9690=CARTESIAN_POINT('Ctrl Pts',(-37.4433111886304,-31.5229768457881,9.52708315354102));
#9691=CARTESIAN_POINT('Ctrl Pts',(-39.8932382226691,-32.9737060147045,9.36829843431533));
#9692=CARTESIAN_POINT('Ctrl Pts',(-42.4406503065726,-31.7023698849862,9.20951371508964));
#9693=CARTESIAN_POINT('Ctrl Pts',(-42.753814324548,-28.8723853155873,9.05072899586397));
#9694=CARTESIAN_POINT('Ctrl Pts',(-40.545843244935,-27.0747919371282,8.89194427663828));
#9695=CARTESIAN_POINT('Ctrl Pts',(-37.838193522748,-27.9551388762876,8.7331595574126));
#9696=CARTESIAN_POINT('Ctrl Pts',(-37.1096259814502,-30.7075420930358,8.57437483818691));
#9697=CARTESIAN_POINT('Ctrl Pts',(-39.0271560874564,-32.8121923488093,8.41559011896123));
#9698=CARTESIAN_POINT('Ctrl Pts',(-41.8353047292891,-32.3423319026381,8.25680539973555));
#9699=CARTESIAN_POINT('Ctrl Pts',(-42.9632642097323,-29.7281028204567,8.09802068050986));
#9700=CARTESIAN_POINT('Ctrl Pts',(-41.3784032552214,-27.3627923526256,7.93923596128418));
#9701=CARTESIAN_POINT('Ctrl Pts',(-38.5316373921794,-27.4118013015827,7.78045124205849));
#9702=CARTESIAN_POINT('Ctrl Pts',(-37.0291329893315,-29.8302637143654,7.62166652283281));
#9703=CARTESIAN_POINT('Ctrl Pts',(-38.2464083841756,-32.4041167373455,7.46288180360713));
#9704=CARTESIAN_POINT('Ctrl Pts',(-41.0690678724485,-32.7770406791433,7.30409708438144));
#9705=CARTESIAN_POINT('Ctrl Pts',(-42.9130134151458,-30.60762971468,7.14531236515577));
#9706=CARTESIAN_POINT('Ctrl Pts',(-42.0901432811058,-27.8819438034811,6.98652764593007));
#9707=CARTESIAN_POINT('Ctrl Pts',(-39.353781508581,-27.0953033418645,6.8277429267044));
#9708=CARTESIAN_POINT('Ctrl Pts',(-37.2090220859903,-28.9678646924366,6.66895820747871));
#9709=CARTESIAN_POINT('Ctrl Pts',(-37.6193568409732,-31.7853288645994,6.51017348825303));
#9710=CARTESIAN_POINT('Ctrl Pts',(-40.209131080766,-32.968353954627,6.35138876902734));
#9711=CARTESIAN_POINT('Ctrl Pts',(-42.6074492712894,-31.433900033371,6.19260404980166));
#9712=CARTESIAN_POINT('Ctrl Pts',(-42.6186907266382,-28.5867343187326,6.03381933057598));
#9713=CARTESIAN_POINT('Ctrl Pts',(-40.2325640805136,-27.0333899891419,5.87503461135029));
#9714=CARTESIAN_POINT('Ctrl Pts',(-37.6335288603857,-28.1959281185863,5.71624989212461));
#9715=CARTESIAN_POINT('Ctrl Pts',(-37.2009588764289,-31.0100642536271,5.55746517289893));
#9716=CARTESIAN_POINT('Ctrl Pts',(-39.3308648032049,-32.8995032499315,5.39868045367324));
#9717=CARTESIAN_POINT('Ctrl Pts',(-42.0733529490857,-32.1344949183462,5.23989573444756));
#9718=CARTESIAN_POINT('Ctrl Pts',(-42.917720720178,-29.4153917491414,5.08111101522188));
#9719=CARTESIAN_POINT('Ctrl Pts',(-41.0909633703201,-27.2314877763366,4.92232629599619));
#9720=CARTESIAN_POINT('Ctrl Pts',(-38.2654470767611,-27.5821110107408,4.76354157677051));
#9721=CARTESIAN_POINT('Ctrl Pts',(-37.0278853310234,-30.1462716732285,4.60475685754483));
#9722=CARTESIAN_POINT('Ctrl Pts',(-38.5112454678223,-32.5765230352142,4.44597213831914));
#9723=CARTESIAN_POINT('Ctrl Pts',(-41.3575357858092,-32.6480101204257,4.28718741909346));
#9724=CARTESIAN_POINT('Ctrl Pts',(-42.9610245172894,-30.2952876835567,4.12840269986777));
#9725=CARTESIAN_POINT('Ctrl Pts',(-41.8537442168751,-27.6722342499095,3.96961798064209));
#9726=CARTESIAN_POINT('Ctrl Pts',(-39.0493917083189,-27.1802119084619,3.81083326141641));
#9727=CARTESIAN_POINT('Ctrl Pts',(-37.1153053873985,-29.2696589826413,3.65204854219072));
#9728=CARTESIAN_POINT('Ctrl Pts',(-37.8221093317535,-32.0277211967132,3.49326382296504));
#9729=CARTESIAN_POINT('Ctrl Pts',(-40.5227362054164,-32.929438145227,3.33447910373936));
#9730=CARTESIAN_POINT('Ctrl Pts',(-42.7448067191771,-31.1493028762435,3.17569438451367));
#9731=CARTESIAN_POINT('Ctrl Pts',(-42.454052021547,-28.3169997845931,3.01690966528799));
#9732=CARTESIAN_POINT('Ctrl Pts',(-39.916653241041,-27.0254556383127,2.8581249460623));
#9733=CARTESIAN_POINT('Ctrl Pts',(-37.4555570337349,-28.4570576183267,2.69934022683662));
#9734=CARTESIAN_POINT('Ctrl Pts',(-37.3238563455092,-31.3011980598908,2.54055550761094));
#9735=CARTESIAN_POINT('Ctrl Pts',(-39.6421209341153,-32.9541127743498,2.38177078838525));
#9736=CARTESIAN_POINT('Ctrl Pts',(-42.288017957861,-31.9025868383414,2.22298606915957));
#9737=CARTESIAN_POINT('Ctrl Pts',(-42.8392722131655,-29.1092724934004,2.06420134993389));
#9738=CARTESIAN_POINT('Ctrl Pts',(-40.7912199078658,-27.1314076374864,1.9054166307082));
#9739=CARTESIAN_POINT('Ctrl Pts',(-38.0188183517463,-27.7796853697847,1.74663191148252));
#9740=CARTESIAN_POINT('Ctrl Pts',(-37.0601568566748,-30.4606371163975,1.58784719225684));
#9741=CARTESIAN_POINT('Ctrl Pts',(-38.792871219088,-32.7198579311106,1.42906247303115));
#9742=CARTESIAN_POINT('Ctrl Pts',(-41.6306959869831,-32.4891441920118,1.27027775380547));
#9743=CARTESIAN_POINT('Ctrl Pts',(-42.9756376328495,-29.9795592991651,1.11149303457979));
#9744=CARTESIAN_POINT('Ctrl Pts',(-41.5964479263253,-27.4888887803364,0.952708315354102));
#9745=CARTESIAN_POINT('Ctrl Pts',(-38.755705070619,-27.2966971535349,0.793923596128418));
#9746=CARTESIAN_POINT('Ctrl Pts',(-37.05415643862,-29.5801374905816,0.635138876902735));
#9747=CARTESIAN_POINT('Ctrl Pts',(-38.0493539639435,-32.2463504309186,0.47635415767705));
#9748=CARTESIAN_POINT('Ctrl Pts',(-40.8305797366192,-32.8592858406621,0.317569438451369));
#9749=CARTESIAN_POINT('Ctrl Pts',(-42.8509964848744,-30.8479863606262,0.158784719225683));
#9750=CARTESIAN_POINT('Ctrl Pts',(-42.4575265280738,-29.000351103447,0.0529282397418946));
#9751=CARTESIAN_POINT('Ctrl Pts',(-41.9134659966651,-28.364012796625,0.));
#9752=CARTESIAN_POINT('Ctrl Pts',(-41.9134659966651,-28.364012796625,0.));
#9753=CARTESIAN_POINT('Ctrl Pts',(-41.97507870596,-28.4219136142157,-2.29978767839653E-16));
#9754=CARTESIAN_POINT('Ctrl Pts',(-42.0333202365815,-28.4829649481258,-3.12714122755679E-15));
#9755=CARTESIAN_POINT('Ctrl Pts',(-42.0881937026029,-28.5467819994154,-2.99760216648792E-15));
#9756=CARTESIAN_POINT('Ctrl Pts',(-42.1445198537573,-28.6122885026088,-2.86463377095567E-15));
#9757=CARTESIAN_POINT('Ctrl Pts',(-42.1972976877423,-28.680709529004,1.07456140052229E-15));
#9758=CARTESIAN_POINT('Ctrl Pts',(-42.24650502312,-28.7516774566258,1.11022302462516E-16));
#9759=CARTESIAN_POINT('Ctrl Pts',(-42.2974066658948,-28.825088952545,-8.8569338215283E-16));
#9760=CARTESIAN_POINT('Ctrl Pts',(-42.3444882808169,-28.9012262809001,-8.80673490056425E-16));
#9761=CARTESIAN_POINT('Ctrl Pts',(-42.3876903859773,-28.97972651679,-1.16573417585641E-15));
#9762=CARTESIAN_POINT('Ctrl Pts',(-42.406591306985,-29.0140703699918,-1.29044822589391E-15));
#9763=CARTESIAN_POINT('Ctrl Pts',(-42.4247491715561,-29.0488670047462,-1.72595682164476E-16));
#9764=CARTESIAN_POINT('Ctrl Pts',(-42.442156553419,-29.0840881184884,-3.33066907387547E-16));
#9765=CARTESIAN_POINT('Ctrl Pts',(-42.4516647905079,-29.1033265486346,-4.20719287704412E-16));
#9766=CARTESIAN_POINT('Ctrl Pts',(-42.4609490902037,-29.1226916438214,-1.13385884475685E-15));
#9767=CARTESIAN_POINT('Ctrl Pts',(-42.4700080385928,-29.1421789203223,-1.33226762955019E-15));
#9768=CARTESIAN_POINT('Ctrl Pts',(-42.4786580277956,-29.1607864588671,-1.52171940391727E-15));
#9769=CARTESIAN_POINT('Ctrl Pts',(-42.4871050433881,-29.1795113953271,-3.9883529154072E-15));
#9770=CARTESIAN_POINT('Ctrl Pts',(-42.4953337543378,-29.1983170459912,-3.88578058618805E-15));
#9771=CARTESIAN_POINT('Ctrl Pts',(-42.5318945025042,-29.2818718897858,-3.43004443014503E-15));
#9772=CARTESIAN_POINT('Ctrl Pts',(-42.5641950342821,-29.3671101952375,-2.5754712386216E-15));
#9773=CARTESIAN_POINT('Ctrl Pts',(-42.5922110799965,-29.4536331140717,-2.35922392732846E-15));
#9774=CARTESIAN_POINT('Ctrl Pts',(-42.6206894211336,-29.5415837557814,-2.139408298678E-15));
#9775=CARTESIAN_POINT('Ctrl Pts',(-42.6447412041289,-29.6308625113997,-3.93501828575153E-15));
#9776=CARTESIAN_POINT('Ctrl Pts',(-42.6643018301641,-29.7210875893022,-5.10702591327572E-15));
#9777=CARTESIAN_POINT('Ctrl Pts',(-42.6835241892463,-29.8097523816524,-6.25876571049136E-15));
#9778=CARTESIAN_POINT('Ctrl Pts',(-42.6984096404725,-29.8993319586104,-3.13934285479542E-15));
#9779=CARTESIAN_POINT('Ctrl Pts',(-42.7088541783029,-29.9894868403159,-3.69149155687865E-15));
#9780=CARTESIAN_POINT('Ctrl Pts',(-42.7129843170356,-30.0251372611314,-3.90983063302867E-15));
#9781=CARTESIAN_POINT('Ctrl Pts',(-42.7164195379488,-30.0608778227311,-2.05747673366752E-15));
#9782=CARTESIAN_POINT('Ctrl Pts',(-42.7191513809188,-30.0966880684131,-1.99840144432528E-15));
#9783=CARTESIAN_POINT('Ctrl Pts',(-42.7207682803523,-30.1178831248609,-1.96343647638277E-15));
#9784=CARTESIAN_POINT('Ctrl Pts',(-42.7221387557394,-30.1391025965479,-2.80327539784527E-15));
#9785=CARTESIAN_POINT('Ctrl Pts',(-42.7232608505681,-30.1603422648391,-3.08086889333481E-15));
#9786=CARTESIAN_POINT('Ctrl Pts',(-42.72400775337,-30.1744800786414,-3.26564414962369E-15));
#9787=CARTESIAN_POINT('Ctrl Pts',(-42.7246445276711,-30.1886268373637,-4.89221388773611E-16));
#9788=CARTESIAN_POINT('Ctrl Pts',(-42.7251702454122,-30.2027667406769,-6.10622663543836E-16));
#9789=CARTESIAN_POINT('Ctrl Pts',(-42.7287089699826,-30.2979456158974,-1.42780199830197E-15));
#9790=CARTESIAN_POINT('Ctrl Pts',(-42.7272289680734,-30.3929754547405,1.61702128845623E-15));
#9791=CARTESIAN_POINT('Ctrl Pts',(-42.7206715932526,-30.4874575333237,1.08246744900953E-15));
#9792=CARTESIAN_POINT('Ctrl Pts',(-42.7141367060633,-30.5816155983765,5.49746789773547E-16));
#9793=CARTESIAN_POINT('Ctrl Pts',(-42.7025595698505,-30.675230607113,-3.71437912378399E-15));
#9794=CARTESIAN_POINT('Ctrl Pts',(-42.6858341417982,-30.7679258265936,-4.91273688396632E-15));
#9795=CARTESIAN_POINT('Ctrl Pts',(-42.6838972772188,-30.7786602656003,-5.05151101230811E-15));
#9796=CARTESIAN_POINT('Ctrl Pts',(-42.6818913149789,-30.7893823802406,-1.99705768075859E-15));
#9797=CARTESIAN_POINT('Ctrl Pts',(-42.6798160451629,-30.8000915919209,-1.99840144432528E-15));
#9798=CARTESIAN_POINT('Ctrl Pts',(-42.662271111955,-30.8906303749705,-2.01079479026814E-15));
#9799=CARTESIAN_POINT('Ctrl Pts',(-42.639776801042,-30.9802472256389,-1.59062155688729E-16));
#9800=CARTESIAN_POINT('Ctrl Pts',(-42.6126084037943,-31.0687042177952,1.11022302462516E-15));
#9801=CARTESIAN_POINT('Ctrl Pts',(-42.6018601180323,-31.1036993270272,1.61237409769298E-15));
#9802=CARTESIAN_POINT('Ctrl Pts',(-42.5903796970892,-31.1385128525821,-4.92893737492136E-16));
#9803=CARTESIAN_POINT('Ctrl Pts',(-42.5781819927525,-31.1731297199112,-6.66133814775094E-16));
#9804=CARTESIAN_POINT('Ctrl Pts',(-42.5722275134488,-31.190028425961,-7.50703371986377E-16));
#9805=CARTESIAN_POINT('Ctrl Pts',(-42.5661020845814,-31.2068802633122,-2.00401734812381E-15));
#9806=CARTESIAN_POINT('Ctrl Pts',(-42.5598073328338,-31.2236834501749,-2.02615701994091E-15));
#9807=CARTESIAN_POINT('Ctrl Pts',(-42.5545628516665,-31.2376830486637,-2.04460271828635E-15));
#9808=CARTESIAN_POINT('Ctrl Pts',(-42.5492037320733,-31.2516410674552,2.43968211885899E-16));
#9809=CARTESIAN_POINT('Ctrl Pts',(-42.5437331875382,-31.2655519281032,1.38777878078145E-16));
#9810=CARTESIAN_POINT('Ctrl Pts',(-42.5095085757547,-31.3525805231897,-5.19309870738232E-16));
#9811=CARTESIAN_POINT('Ctrl Pts',(-42.4709055243979,-31.4378209883345,4.76536274428084E-16));
#9812=CARTESIAN_POINT('Ctrl Pts',(-42.4282565184601,-31.5210414522706,3.33066907387547E-16));
#9813=CARTESIAN_POINT('Ctrl Pts',(-42.3840273012413,-31.6073453624215,1.84281779585565E-16));
#9814=CARTESIAN_POINT('Ctrl Pts',(-42.3354466279213,-31.6914775359273,4.72784736073334E-16));
#9815=CARTESIAN_POINT('Ctrl Pts',(-42.2828293656982,-31.7731758332943,4.85722573273506E-16));
#9816=CARTESIAN_POINT('Ctrl Pts',(-42.229634476967,-31.8557710055697,4.98802440625183E-16));
#9817=CARTESIAN_POINT('Ctrl Pts',(-42.1723134681871,-31.9358793885275,-6.12161291006381E-16));
#9818=CARTESIAN_POINT('Ctrl Pts',(-42.1111400734139,-32.0132147571248,-4.85722573273506E-16));
#9819=CARTESIAN_POINT('Ctrl Pts',(-42.0873228863003,-32.0433244306392,-4.36495051900537E-16));
#9820=CARTESIAN_POINT('Ctrl Pts',(-42.0629212212804,-32.0730135273603,-5.06570471742106E-15));
#9821=CARTESIAN_POINT('Ctrl Pts',(-42.0379493675179,-32.1022641150462,-5.35682609381638E-15));
#9822=CARTESIAN_POINT('Ctrl Pts',(-42.0179603023369,-32.1256781518813,-5.58985821965319E-15));
#9823=CARTESIAN_POINT('Ctrl Pts',(-41.997605872731,-32.1488112067583,-9.77501083290033E-16));
#9824=CARTESIAN_POINT('Ctrl Pts',(-41.9768929709471,-32.1716537402857,-1.08246744900953E-15));
#9825=CARTESIAN_POINT('Ctrl Pts',(-41.9653469750443,-32.184386857126,-1.14097886576662E-15));
#9826=CARTESIAN_POINT('Ctrl Pts',(-41.9536946662295,-32.1970240341331,-1.52433067033023E-15));
#9827=CARTESIAN_POINT('Ctrl Pts',(-41.9419422851552,-32.2095588617621,-1.346145417358E-15));
#9828=CARTESIAN_POINT('Ctrl Pts',(-41.8728869093774,-32.2832117859446,-2.99153363207995E-16));
#9829=CARTESIAN_POINT('Ctrl Pts',(-41.8003309454798,-32.3533872730139,-3.08633678840453E-15));
#9830=CARTESIAN_POINT('Ctrl Pts',(-41.7245863310056,-32.4197964723545,-1.84574577843932E-15));
#9831=CARTESIAN_POINT('Ctrl Pts',(-41.6603355224085,-32.4761284609128,-7.93407257979879E-16));
#9832=CARTESIAN_POINT('Ctrl Pts',(-41.5937892971726,-32.5297504849909,-1.35961820572097E-15));
#9833=CARTESIAN_POINT('Ctrl Pts',(-41.5251131887883,-32.5804713188053,-2.43555176027144E-15));
#9834=CARTESIAN_POINT('Ctrl Pts',(-41.502422805649,-32.5972293323193,-2.79103702522908E-15));
#9835=CARTESIAN_POINT('Ctrl Pts',(-41.4794997526171,-32.6136705085288,1.28421174174714E-15));
#9836=CARTESIAN_POINT('Ctrl Pts',(-41.456349528936,-32.6297875098032,1.76941794549634E-15));
#9837=CARTESIAN_POINT('Ctrl Pts',(-41.4397562694643,-32.6413396048385,2.11719654785573E-15));
#9838=CARTESIAN_POINT('Ctrl Pts',(-41.4230453329585,-32.6527256775375,-2.01867653155568E-16));
#9839=CARTESIAN_POINT('Ctrl Pts',(-41.4062333015004,-32.663933539865,-3.33066907387547E-16));
#9840=CARTESIAN_POINT('Ctrl Pts',(-41.3198795013252,-32.721501925115,-1.00696251668964E-15));
#9841=CARTESIAN_POINT('Ctrl Pts',(-41.2307763067095,-32.7744320587763,-3.13830639635427E-15));
#9842=CARTESIAN_POINT('Ctrl Pts',(-41.139232260598,-32.8224024784536,-3.40005801291454E-15));
#9843=CARTESIAN_POINT('Ctrl Pts',(-41.0476882144866,-32.870372898131,-3.66180962947481E-15));
#9844=CARTESIAN_POINT('Ctrl Pts',(-40.9537026715522,-32.9133845145118,-1.77753300593033E-15));
#9845=CARTESIAN_POINT('Ctrl Pts',(-40.857546131199,-32.9510751186699,-1.72127936903799E-15));
#9846=CARTESIAN_POINT('Ctrl Pts',(-40.8369781689331,-32.9591371695845,-1.70558910776797E-15));
#9847=CARTESIAN_POINT('Ctrl Pts',(-40.8163107577518,-32.966955588126,-7.07161017401445E-17));
#9848=CARTESIAN_POINT('Ctrl Pts',(-40.7955478019229,-32.974531551058,2.77555756156289E-17));
#9849=CARTESIAN_POINT('Ctrl Pts',(-42.5142225916618,-29.9985870806183,9.11258330249199));
#9850=CARTESIAN_POINT('Ctrl Pts',(-42.5159019272474,-29.6714493029011,9.09196520028265));
#9851=CARTESIAN_POINT('Ctrl Pts',(-42.4566449317272,-29.3448946486763,9.07134709807331));
#9852=CARTESIAN_POINT('Ctrl Pts',(-42.3336251416166,-29.0444505140773,9.05072899586397));
#9853=CARTESIAN_POINT('Ctrl Pts',(-42.017823964677,-28.2731875227676,8.99780075612208));
#9854=CARTESIAN_POINT('Ctrl Pts',(-41.281833604806,-27.6739897299479,8.94487251638018));
#9855=CARTESIAN_POINT('Ctrl Pts',(-40.4625634711727,-27.521115323398,8.89194427663829));
#9856=CARTESIAN_POINT('Ctrl Pts',(-39.6432933375393,-27.368240916848,8.83901603689639));
#9857=CARTESIAN_POINT('Ctrl Pts',(-38.7407434301437,-27.6616898965678,8.7860877971545));
#9858=CARTESIAN_POINT('Ctrl Pts',(-38.1680405528962,-28.2671482558857,8.7331595574126));
#9859=CARTESIAN_POINT('Ctrl Pts',(-37.5953376756488,-28.8726066152036,8.68023131767071));
#9860=CARTESIAN_POINT('Ctrl Pts',(-37.3524818285495,-29.7900743541197,8.62730307792881));
#9861=CARTESIAN_POINT('Ctrl Pts',(-37.5506422560009,-30.5995832662067,8.57437483818692));
#9862=CARTESIAN_POINT('Ctrl Pts',(-37.7488026834523,-31.4090921782936,8.52144659844502));
#9863=CARTESIAN_POINT('Ctrl Pts',(-38.3879793854543,-32.1106422635514,8.46851835870313));
#9864=CARTESIAN_POINT('Ctrl Pts',(-39.1755925100941,-32.3831072318185,8.41559011896124));
#9865=CARTESIAN_POINT('Ctrl Pts',(-39.963205634734,-32.6555722000855,8.36266187921934));
#9866=CARTESIAN_POINT('Ctrl Pts',(-40.8992551820115,-32.4989520513618,8.30973363947745));
#9867=CARTESIAN_POINT('Ctrl Pts',(-41.5552732023909,-31.9849371299697,8.25680539973555));
#9868=CARTESIAN_POINT('Ctrl Pts',(-42.1511258460839,-31.518064055916,8.20873136732103));
#9869=CARTESIAN_POINT('Ctrl Pts',(-42.5159566006121,-30.7563455532992,8.16065733490651));
#9870=CARTESIAN_POINT('Ctrl Pts',(-42.5208030005754,-29.9986726513939,8.11258330249199));
#9871=CARTESIAN_POINT('Ctrl Pts',(-40.7937992825329,-32.9692229537457,10.));
#9872=CARTESIAN_POINT('Ctrl Pts',(-40.8868533728222,-32.935183351848,10.));
#9873=CARTESIAN_POINT('Ctrl Pts',(-40.9778402395471,-32.8963743016634,10.));
#9874=CARTESIAN_POINT('Ctrl Pts',(-41.0665521014268,-32.8531245323668,10.));
#9875=CARTESIAN_POINT('Ctrl Pts',(-41.1572337566638,-32.8089144280433,10.));
#9876=CARTESIAN_POINT('Ctrl Pts',(-41.245538922155,-32.7600635910313,10.));
#9877=CARTESIAN_POINT('Ctrl Pts',(-41.3312167295181,-32.7068775848614,10.));
#9878=CARTESIAN_POINT('Ctrl Pts',(-41.414166125894,-32.6553852878102,10.));
#9879=CARTESIAN_POINT('Ctrl Pts',(-41.4946531615533,-32.5998286696066,10.));
#9880=CARTESIAN_POINT('Ctrl Pts',(-41.5724164694193,-32.540454332485,10.));
#9881=CARTESIAN_POINT('Ctrl Pts',(-41.6404593638021,-32.4885017875035,10.));
#9882=CARTESIAN_POINT('Ctrl Pts',(-41.706416607328,-32.4336255845195,10.));
#9883=CARTESIAN_POINT('Ctrl Pts',(-41.7700878401902,-32.375977951992,10.));
#9884=CARTESIAN_POINT('Ctrl Pts',(-41.7834304287881,-32.3638976354993,10.));
#9885=CARTESIAN_POINT('Ctrl Pts',(-41.7966744017855,-32.3516937148243,10.));
#9886=CARTESIAN_POINT('Ctrl Pts',(-41.8098007360623,-32.3393838948222,10.));
#9887=CARTESIAN_POINT('Ctrl Pts',(-41.8822283307573,-32.2714616070702,10.));
#9888=CARTESIAN_POINT('Ctrl Pts',(-41.9511902075176,-32.2002181058656,10.));
#9889=CARTESIAN_POINT('Ctrl Pts',(-42.0164470228621,-32.125944563464,10.));
#9890=CARTESIAN_POINT('Ctrl Pts',(-42.081342504664,-32.0520822811284,10.));
#9891=CARTESIAN_POINT('Ctrl Pts',(-42.142574327181,-31.9752226218996,10.));
#9892=CARTESIAN_POINT('Ctrl Pts',(-42.199863486846,-31.8956252027112,10.));
#9893=CARTESIAN_POINT('Ctrl Pts',(-42.2557185827112,-31.8180202682806,10.));
#9894=CARTESIAN_POINT('Ctrl Pts',(-42.3078262008549,-31.7378121817919,10.));
#9895=CARTESIAN_POINT('Ctrl Pts',(-42.3558809073996,-31.6552274273718,10.));
#9896=CARTESIAN_POINT('Ctrl Pts',(-42.3766084917365,-31.6196058913086,10.));
#9897=CARTESIAN_POINT('Ctrl Pts',(-42.3965814143594,-31.5835420633842,10.));
#9898=CARTESIAN_POINT('Ctrl Pts',(-42.4157721815743,-31.5470537860881,10.));
#9899=CARTESIAN_POINT('Ctrl Pts',(-42.4294375496695,-31.5210712010862,10.));
#9900=CARTESIAN_POINT('Ctrl Pts',(-42.4427062812236,-31.4948733921638,10.));
#9901=CARTESIAN_POINT('Ctrl Pts',(-42.4555678526521,-31.4684667979364,10.));
#9902=CARTESIAN_POINT('Ctrl Pts',(-42.4611833574038,-31.4569373859838,10.));
#9903=CARTESIAN_POINT('Ctrl Pts',(-42.4667203177096,-31.4453699707948,10.));
#9904=CARTESIAN_POINT('Ctrl Pts',(-42.4721741634146,-31.4337733648849,10.));
#9905=CARTESIAN_POINT('Ctrl Pts',(-42.5124020023045,-31.3482362192731,10.));
#9906=CARTESIAN_POINT('Ctrl Pts',(-42.5481738032464,-31.2609859402736,10.));
#9907=CARTESIAN_POINT('Ctrl Pts',(-42.5792385873022,-31.1722598487437,10.));
#9908=CARTESIAN_POINT('Ctrl Pts',(-42.6096166607224,-31.085495114827,10.));
#9909=CARTESIAN_POINT('Ctrl Pts',(-42.6354937388761,-30.997318420516,10.));
#9910=CARTESIAN_POINT('Ctrl Pts',(-42.6565860035544,-30.9079428775445,10.));
#9911=CARTESIAN_POINT('Ctrl Pts',(-42.6603146693337,-30.8921431740198,10.));
#9912=CARTESIAN_POINT('Ctrl Pts',(-42.6638936748766,-30.8763059973636,10.));
#9913=CARTESIAN_POINT('Ctrl Pts',(-42.6673212800257,-30.8604325193031,10.));
#9914=CARTESIAN_POINT('Ctrl Pts',(-42.6874321817243,-30.7672975335032,10.));
#9915=CARTESIAN_POINT('Ctrl Pts',(-42.7023351154996,-30.6729118079479,10.));
#9916=CARTESIAN_POINT('Ctrl Pts',(-42.7121085725822,-30.5776842387582,10.));
#9917=CARTESIAN_POINT('Ctrl Pts',(-42.7153864632551,-30.5457461478441,10.));
#9918=CARTESIAN_POINT('Ctrl Pts',(-42.7180869507972,-30.5137134838219,10.));
#9919=CARTESIAN_POINT('Ctrl Pts',(-42.7202117715535,-30.4816021420478,10.));
#9920=CARTESIAN_POINT('Ctrl Pts',(-42.7214003930878,-30.4636391057704,10.));
#9921=CARTESIAN_POINT('Ctrl Pts',(-42.7224088624834,-30.4456514543982,10.));
#9922=CARTESIAN_POINT('Ctrl Pts',(-42.723237404335,-30.427642015416,10.));
#9923=CARTESIAN_POINT('Ctrl Pts',(-42.7238116710756,-30.4151595779797,10.));
#9924=CARTESIAN_POINT('Ctrl Pts',(-42.7242993863234,-30.4026682033291,10.));
#9925=CARTESIAN_POINT('Ctrl Pts',(-42.7247004999338,-30.3901783131038,10.));
#9926=CARTESIAN_POINT('Ctrl Pts',(-42.7276933286286,-30.296987504066,10.));
#9927=CARTESIAN_POINT('Ctrl Pts',(-42.7258765702513,-30.2037322455153,10.));
#9928=CARTESIAN_POINT('Ctrl Pts',(-42.7193893277119,-30.1107876657792,10.));
#9929=CARTESIAN_POINT('Ctrl Pts',(-42.7128891265852,-30.0176574246571,10.));
#9930=CARTESIAN_POINT('Ctrl Pts',(-42.70169938016,-29.9248381231515,10.));
#9931=CARTESIAN_POINT('Ctrl Pts',(-42.6859089810961,-29.8327191439709,10.));
#9932=CARTESIAN_POINT('Ctrl Pts',(-42.6703416896879,-29.7419017436428,10.));
#9933=CARTESIAN_POINT('Ctrl Pts',(-42.6503023675462,-29.6517641681989,10.));
#9934=CARTESIAN_POINT('Ctrl Pts',(-42.625833145288,-29.5627046786781,10.));
#9935=CARTESIAN_POINT('Ctrl Pts',(-42.6163194806669,-29.5280782362974,10.));
#9936=CARTESIAN_POINT('Ctrl Pts',(-42.6061357356979,-29.4936151031392,10.));
#9937=CARTESIAN_POINT('Ctrl Pts',(-42.5952828198538,-29.4593401489932,10.));
#9938=CARTESIAN_POINT('Ctrl Pts',(-42.5894786042462,-29.4410096628213,10.));
#9939=CARTESIAN_POINT('Ctrl Pts',(-42.5834829790806,-29.422733014913,10.));
#9940=CARTESIAN_POINT('Ctrl Pts',(-42.5772959877695,-29.4045141238123,10.));
#9941=CARTESIAN_POINT('Ctrl Pts',(-42.5718473975396,-29.3884696092719,10.));
#9942=CARTESIAN_POINT('Ctrl Pts',(-42.566249914374,-29.3724688136786,10.));
#9943=CARTESIAN_POINT('Ctrl Pts',(-42.560509689398,-29.3565308232038,10.));
#9944=CARTESIAN_POINT('Ctrl Pts',(-42.528084217673,-29.2665000558295,10.));
#9945=CARTESIAN_POINT('Ctrl Pts',(-42.4910677016941,-29.1783480221378,10.));
#9946=CARTESIAN_POINT('Ctrl Pts',(-42.4495331756161,-29.0925192906336,10.));
#9947=CARTESIAN_POINT('Ctrl Pts',(-42.4183822810576,-29.0281477420054,10.));
#9948=CARTESIAN_POINT('Ctrl Pts',(-42.3846888574719,-28.965083587818,10.));
#9949=CARTESIAN_POINT('Ctrl Pts',(-42.3484663478005,-28.9035315373059,10.));
#9950=CARTESIAN_POINT('Ctrl Pts',(-42.3335345656046,-28.8781583144039,10.));
#9951=CARTESIAN_POINT('Ctrl Pts',(-42.3181728564796,-28.8530422408006,10.));
#9952=CARTESIAN_POINT('Ctrl Pts',(-42.3023815042107,-28.8281985617541,10.));
#9953=CARTESIAN_POINT('Ctrl Pts',(-42.2929488646612,-28.813358700953,10.));
#9954=CARTESIAN_POINT('Ctrl Pts',(-42.2833676059461,-28.7986234509943,10.));
#9955=CARTESIAN_POINT('Ctrl Pts',(-42.2736397669503,-28.7839981335806,10.));
#9956=CARTESIAN_POINT('Ctrl Pts',(-42.2261110872739,-28.7125411505014,10.));
#9957=CARTESIAN_POINT('Ctrl Pts',(-42.1750736185291,-28.6436861425009,10.));
#9958=CARTESIAN_POINT('Ctrl Pts',(-42.1205617426708,-28.5777858210467,10.));
#9959=CARTESIAN_POINT('Ctrl Pts',(-42.0689757131425,-28.5154226043176,10.));
#9960=CARTESIAN_POINT('Ctrl Pts',(-42.0142777437963,-28.4557051898554,10.));
#9961=CARTESIAN_POINT('Ctrl Pts',(-41.9564731814538,-28.3989683641584,10.));
#9962=CARTESIAN_POINT('Ctrl Pts',(-41.9435072079919,-28.3862418916018,10.));
#9963=CARTESIAN_POINT('Ctrl Pts',(-41.9303848447124,-28.3736655421759,10.));
#9964=CARTESIAN_POINT('Ctrl Pts',(-41.9171093217587,-28.3612406458478,10.));
#9965=CARTESIAN_POINT('Origin',(0.,0.,10.));
#9966=CARTESIAN_POINT('',(-60.,50.,10.));
#9967=CARTESIAN_POINT('',(-60.,-50.,10.));
#9968=CARTESIAN_POINT('',(-60.,50.,10.));
#9969=CARTESIAN_POINT('',(60.,-50.,10.));
#9970=CARTESIAN_POINT('',(-60.,-50.,10.));
#9971=CARTESIAN_POINT('',(60.,50.,10.));
#9972=CARTESIAN_POINT('',(60.,-50.,10.));
#9973=CARTESIAN_POINT('',(60.,50.,10.));
#9974=CARTESIAN_POINT('Ctrl Pts',(41.9134659966651,-28.364012796625,10.));
#9975=CARTESIAN_POINT('Ctrl Pts',(41.9750786768602,-28.4219135868691,10.));
#9976=CARTESIAN_POINT('Ctrl Pts',(42.0333201769005,-28.4829648953928,10.));
#9977=CARTESIAN_POINT('Ctrl Pts',(42.0881936118187,-28.5467819227993,10.));
#9978=CARTESIAN_POINT('Ctrl Pts',(42.1445197342576,-28.612288405212,10.));
#9979=CARTESIAN_POINT('Ctrl Pts',(42.1972975385705,-28.6807094127424,10.));
#9980=CARTESIAN_POINT('Ctrl Pts',(42.2465048443317,-28.7516773228468,10.));
#9981=CARTESIAN_POINT('Ctrl Pts',(42.2974064829938,-28.8250888388982,10.));
#9982=CARTESIAN_POINT('Ctrl Pts',(42.3444880898825,-28.901226191665,10.));
#9983=CARTESIAN_POINT('Ctrl Pts',(42.3876901841144,-28.9797264550545,10.));
#9984=CARTESIAN_POINT('Ctrl Pts',(42.4065911003408,-29.0140703202873,10.));
#9985=CARTESIAN_POINT('Ctrl Pts',(42.4247489595759,-29.0488669676648,10.));
#9986=CARTESIAN_POINT('Ctrl Pts',(42.442156335631,-29.0840880945258,10.));
#9987=CARTESIAN_POINT('Ctrl Pts',(42.4516645839391,-29.1033265609567,10.));
#9988=CARTESIAN_POINT('Ctrl Pts',(42.4609488940356,-29.1226916929596,10.));
#9989=CARTESIAN_POINT('Ctrl Pts',(42.4700078520136,-29.1421790067722,10.));
#9990=CARTESIAN_POINT('Ctrl Pts',(42.4786578515885,-29.1607865835603,10.));
#9991=CARTESIAN_POINT('Ctrl Pts',(42.4871048767656,-29.1795115587778,10.));
#9992=CARTESIAN_POINT('Ctrl Pts',(42.4953335964791,-29.1983172485575,10.));
#9993=CARTESIAN_POINT('Ctrl Pts',(42.5318943081609,-29.2818720937771,10.));
#9994=CARTESIAN_POINT('Ctrl Pts',(42.5641948048895,-29.3671104009095,10.));
#9995=CARTESIAN_POINT('Ctrl Pts',(42.592210818053,-29.4536333209677,10.));
#9996=CARTESIAN_POINT('Ctrl Pts',(42.6206891306107,-29.5415839778454,10.));
#9997=CARTESIAN_POINT('Ctrl Pts',(42.644740886205,-29.6308627485803,10.));
#9998=CARTESIAN_POINT('Ctrl Pts',(42.6643014871103,-29.7210878406195,10.));
#9999=CARTESIAN_POINT('Ctrl Pts',(42.6835238259951,-29.8097526676095,10.));
#10000=CARTESIAN_POINT('Ctrl Pts',(42.698409257187,-29.89933227869,10.));
#10001=CARTESIAN_POINT('Ctrl Pts',(42.7088537761227,-29.9894871928845,10.));
#10002=CARTESIAN_POINT('Ctrl Pts',(42.7129839090531,-30.0251376409564,10.));
#10003=CARTESIAN_POINT('Ctrl Pts',(42.7164191237806,-30.0608782296299,10.));
#10004=CARTESIAN_POINT('Ctrl Pts',(42.7191509602312,-30.0966885021091,10.));
#10005=CARTESIAN_POINT('Ctrl Pts',(42.7207678549321,-30.1178835629617,10.));
#10006=CARTESIAN_POINT('Ctrl Pts',(42.7221383257361,-30.1391030389302,10.));
#10007=CARTESIAN_POINT('Ctrl Pts',(42.7232604161444,-30.1603427113668,10.));
#10008=CARTESIAN_POINT('Ctrl Pts',(42.7240073161938,-30.1744805315225,10.));
#10009=CARTESIAN_POINT('Ctrl Pts',(42.7246440877591,-30.1886272965526,10.));
#10010=CARTESIAN_POINT('Ctrl Pts',(42.7251698027865,-30.2027672061038,10.));
#10011=CARTESIAN_POINT('Ctrl Pts',(42.7287085081136,-30.2979460970433,10.));
#10012=CARTESIAN_POINT('Ctrl Pts',(42.7272284907081,-30.3929759486328,10.));
#10013=CARTESIAN_POINT('Ctrl Pts',(42.7206711052329,-30.4874580359568,10.));
#10014=CARTESIAN_POINT('Ctrl Pts',(42.714136206117,-30.5816161285794,10.));
#10015=CARTESIAN_POINT('Ctrl Pts',(42.7025590607659,-30.6752311606915,10.));
#10016=CARTESIAN_POINT('Ctrl Pts',(42.6858336273981,-30.7679263980985,10.));
#10017=CARTESIAN_POINT('Ctrl Pts',(42.6838967626779,-30.7786608365503,10.));
#10018=CARTESIAN_POINT('Ctrl Pts',(42.6818908003822,-30.7893829505687,10.));
#10019=CARTESIAN_POINT('Ctrl Pts',(42.6798155305974,-30.8000921615584,10.));
#10020=CARTESIAN_POINT('Ctrl Pts',(42.6622705920295,-30.8906309677886,10.));
#10021=CARTESIAN_POINT('Ctrl Pts',(42.6397762787909,-30.9802478361479,10.));
#10022=CARTESIAN_POINT('Ctrl Pts',(42.6126078815683,-31.0687048411986,10.));
#10023=CARTESIAN_POINT('Ctrl Pts',(42.6018595917985,-31.1036999686133,10.));
#10024=CARTESIAN_POINT('Ctrl Pts',(42.5903791666683,-31.1385135114639,10.));
#10025=CARTESIAN_POINT('Ctrl Pts',(42.5781814579395,-31.173130395225,10.));
#10026=CARTESIAN_POINT('Ctrl Pts',(42.5722268554977,-31.1900294526755,10.));
#10027=CARTESIAN_POINT('Ctrl Pts',(42.5661012964961,-31.2068816393169,10.));
#10028=CARTESIAN_POINT('Ctrl Pts',(42.5598064077136,-31.223685173253,10.));
#10029=CARTESIAN_POINT('Ctrl Pts',(42.5545620438917,-31.237684442899,10.));
#10030=CARTESIAN_POINT('Ctrl Pts',(42.549203047486,-31.2516421336463,10.));
#10031=CARTESIAN_POINT('Ctrl Pts',(42.5437326312534,-31.265552668785,10.));
#10032=CARTESIAN_POINT('Ctrl Pts',(42.5095080157812,-31.3525812779227,10.));
#10033=CARTESIAN_POINT('Ctrl Pts',(42.4709049618174,-31.4378217521669,10.));
#10034=CARTESIAN_POINT('Ctrl Pts',(42.4282559537337,-31.5210422209145,10.));
#10035=CARTESIAN_POINT('Ctrl Pts',(42.3840267420549,-31.6073461209027,10.));
#10036=CARTESIAN_POINT('Ctrl Pts',(42.335446076298,-31.6914782803964,10.));
#10037=CARTESIAN_POINT('Ctrl Pts',(42.2828288228026,-31.7731765607072,10.));
#10038=CARTESIAN_POINT('Ctrl Pts',(42.2296339485798,-31.8557717069121,10.));
#10039=CARTESIAN_POINT('Ctrl Pts',(42.1723129563808,-31.9358800612183,10.));
#10040=CARTESIAN_POINT('Ctrl Pts',(42.1111395793052,-32.013215399448,10.));
#10041=CARTESIAN_POINT('Ctrl Pts',(42.087322330385,-32.0433251479856,10.));
#10042=CARTESIAN_POINT('Ctrl Pts',(42.0629206003569,-32.0730143170435,10.));
#10043=CARTESIAN_POINT('Ctrl Pts',(42.0379486784512,-32.1022649742732,10.));
#10044=CARTESIAN_POINT('Ctrl Pts',(42.0179581141926,-32.1256807588157,10.));
#10045=CARTESIAN_POINT('Ctrl Pts',(41.9976021306956,-32.1488155190018,10.));
#10046=CARTESIAN_POINT('Ctrl Pts',(41.9768876217174,-32.1716597133009,10.));
#10047=CARTESIAN_POINT('Ctrl Pts',(41.9653431028421,-32.1843911390157,10.));
#10048=CARTESIAN_POINT('Ctrl Pts',(41.9536923027656,-32.1970266455306,10.));
#10049=CARTESIAN_POINT('Ctrl Pts',(41.9419414550198,-32.2095598310127,10.));
#10050=CARTESIAN_POINT('Ctrl Pts',(41.8728860824193,-32.2832127122403,10.));
#10051=CARTESIAN_POINT('Ctrl Pts',(41.8003301222597,-32.3533881546089,10.));
#10052=CARTESIAN_POINT('Ctrl Pts',(41.7245855110489,-32.4197973083236,10.));
#10053=CARTESIAN_POINT('Ctrl Pts',(41.6603347701438,-32.4761292012575,10.));
#10054=CARTESIAN_POINT('Ctrl Pts',(41.593788616895,-32.5297511345173,10.));
#10055=CARTESIAN_POINT('Ctrl Pts',(41.5251125836829,-32.5804718833742,10.));
#10056=CARTESIAN_POINT('Ctrl Pts',(41.5024215392248,-32.5972303755792,10.));
#10057=CARTESIAN_POINT('Ctrl Pts',(41.4794978111518,-32.6136720119584,10.));
#10058=CARTESIAN_POINT('Ctrl Pts',(41.4563468991644,-32.6297894542513,10.));
#10059=CARTESIAN_POINT('Ctrl Pts',(41.4397544793987,-32.6413409373297,10.));
#10060=CARTESIAN_POINT('Ctrl Pts',(41.4230443952104,-32.6527264145468,10.));
#10061=CARTESIAN_POINT('Ctrl Pts',(41.406233226403,-32.6639336995976,10.));
#10062=CARTESIAN_POINT('Ctrl Pts',(41.3198794645924,-32.7215020480517,10.));
#10063=CARTESIAN_POINT('Ctrl Pts',(41.2307763069737,-32.7744321483762,10.));
#10064=CARTESIAN_POINT('Ctrl Pts',(41.1392322953199,-32.8224025393254,10.));
#10065=CARTESIAN_POINT('Ctrl Pts',(41.0476882836661,-32.8703729302747,10.));
#10066=CARTESIAN_POINT('Ctrl Pts',(40.9537027726528,-32.9133845225335,10.));
#10067=CARTESIAN_POINT('Ctrl Pts',(40.8575462605233,-32.95107510836,10.));
#10068=CARTESIAN_POINT('Ctrl Pts',(40.8369783011898,-32.9591371565704,10.));
#10069=CARTESIAN_POINT('Ctrl Pts',(40.8163108927417,-32.9669555725993,10.));
#10070=CARTESIAN_POINT('Ctrl Pts',(40.795547939453,-32.9745315332036,10.));
#10071=CARTESIAN_POINT('Ctrl Pts',(39.2062007174671,-32.9692229537457,10.));
#10072=CARTESIAN_POINT('Ctrl Pts',(39.1131464644267,-32.9351832923129,10.));
#10073=CARTESIAN_POINT('Ctrl Pts',(39.0221594360209,-32.8963742052227,10.));
#10074=CARTESIAN_POINT('Ctrl Pts',(38.9334474159654,-32.8531244154564,10.));
#10075=CARTESIAN_POINT('Ctrl Pts',(38.8427656811494,-32.8089143302392,10.));
#10076=CARTESIAN_POINT('Ctrl Pts',(38.7544604354353,-32.7600635379137,10.));
#10077=CARTESIAN_POINT('Ctrl Pts',(38.6687825492772,-32.7068775946067,10.));
#10078=CARTESIAN_POINT('Ctrl Pts',(38.5858331739442,-32.6553854188348,10.));
#10079=CARTESIAN_POINT('Ctrl Pts',(38.5053461548915,-32.5998289484912,10.));
#10080=CARTESIAN_POINT('Ctrl Pts',(38.4275828602563,-32.5404547782488,10.));
#10081=CARTESIAN_POINT('Ctrl Pts',(38.3595399774506,-32.4885023792867,10.));
#10082=CARTESIAN_POINT('Ctrl Pts',(38.293582742916,-32.4336263368915,10.));
#10083=CARTESIAN_POINT('Ctrl Pts',(38.2299115171604,-32.3759788744261,10.));
#10084=CARTESIAN_POINT('Ctrl Pts',(38.2165690420241,-32.3638986949496,10.));
#10085=CARTESIAN_POINT('Ctrl Pts',(38.2033251808735,-32.3516949139002,10.));
#10086=CARTESIAN_POINT('Ctrl Pts',(38.190198956418,-32.3393852356562,10.));
#10087=CARTESIAN_POINT('Ctrl Pts',(38.1177713352618,-32.2714631370029,10.));
#10088=CARTESIAN_POINT('Ctrl Pts',(38.0488094314203,-32.2002198323416,10.));
#10089=CARTESIAN_POINT('Ctrl Pts',(37.9835525897255,-32.1259464860604,10.));
#10090=CARTESIAN_POINT('Ctrl Pts',(37.9186571141777,-32.0520844357027,10.));
#10091=CARTESIAN_POINT('Ctrl Pts',(37.8574252949744,-31.9752250110449,10.));
#10092=CARTESIAN_POINT('Ctrl Pts',(37.8001361365983,-31.8956278208525,10.));
#10093=CARTESIAN_POINT('Ctrl Pts',(37.7442810137189,-31.8180230704062,10.));
#10094=CARTESIAN_POINT('Ctrl Pts',(37.6921733704247,-31.7378151599815,10.));
#10095=CARTESIAN_POINT('Ctrl Pts',(37.6441186418705,-31.6552305662644,10.));
#10096=CARTESIAN_POINT('Ctrl Pts',(37.6233910600879,-31.6196091202224,10.));
#10097=CARTESIAN_POINT('Ctrl Pts',(37.6034181397275,-31.5835453799715,10.));
#10098=CARTESIAN_POINT('Ctrl Pts',(37.5842273745413,-31.5470571873502,10.));
#10099=CARTESIAN_POINT('Ctrl Pts',(37.5705621606998,-31.5210749531859,10.));
#10100=CARTESIAN_POINT('Ctrl Pts',(37.5572935744113,-31.4948774983938,10.));
#10101=CARTESIAN_POINT('Ctrl Pts',(37.544432138925,-31.4684712611331,10.));
#10102=CARTESIAN_POINT('Ctrl Pts',(37.5388166989825,-31.4569420162363,10.));
#10103=CARTESIAN_POINT('Ctrl Pts',(37.5332798012255,-31.4453747680287,10.));
#10104=CARTESIAN_POINT('Ctrl Pts',(37.5278260160845,-31.4337783295543,10.));
#10105=CARTESIAN_POINT('Ctrl Pts',(37.4875981325696,-31.3482413741973,10.));
#10106=CARTESIAN_POINT('Ctrl Pts',(37.4518262853914,-31.2609912635665,10.));
#10107=CARTESIAN_POINT('Ctrl Pts',(37.4207614540347,-31.1722653110286,10.));
#10108=CARTESIAN_POINT('Ctrl Pts',(37.3903833312938,-31.0855007042761,10.));
#10109=CARTESIAN_POINT('Ctrl Pts',(37.3645062037076,-30.9973241087638,10.));
#10110=CARTESIAN_POINT('Ctrl Pts',(37.3434138900069,-30.9079486289182,10.));
#10111=CARTESIAN_POINT('Ctrl Pts',(37.3396850724138,-30.8921483299862,10.));
#10112=CARTESIAN_POINT('Ctrl Pts',(37.3361059265609,-30.8763105539293,10.));
#10113=CARTESIAN_POINT('Ctrl Pts',(37.3326781928098,-30.8604364725678,10.));
#10114=CARTESIAN_POINT('Ctrl Pts',(37.3125672988369,-30.7673014771556,10.));
#10115=CARTESIAN_POINT('Ctrl Pts',(37.2976643807312,-30.6729157024642,10.));
#10116=CARTESIAN_POINT('Ctrl Pts',(37.2878909459398,-30.5776880515643,10.));
#10117=CARTESIAN_POINT('Ctrl Pts',(37.2846130657184,-30.5457499622357,10.));
#10118=CARTESIAN_POINT('Ctrl Pts',(37.2819125883248,-30.5137172963057,10.));
#10119=CARTESIAN_POINT('Ctrl Pts',(37.2797877773691,-30.4816059493477,10.));
#10120=CARTESIAN_POINT('Ctrl Pts',(37.2785991601696,-30.4636428928259,10.));
#10121=CARTESIAN_POINT('Ctrl Pts',(37.2775906953478,-30.4456552201366,10.));
#10122=CARTESIAN_POINT('Ctrl Pts',(37.2767621583002,-30.4276457588107,10.));
#10123=CARTESIAN_POINT('Ctrl Pts',(37.2761878954323,-30.4151633176917,10.));
#10124=CARTESIAN_POINT('Ctrl Pts',(37.2757001840025,-30.402671938853,10.));
#10125=CARTESIAN_POINT('Ctrl Pts',(37.2752990741519,-30.3901820439812,10.));
#10126=CARTESIAN_POINT('Ctrl Pts',(37.2723062709527,-30.2969911206636,10.));
#10127=CARTESIAN_POINT('Ctrl Pts',(37.2741230598307,-30.2037357219583,10.));
#10128=CARTESIAN_POINT('Ctrl Pts',(37.2806103365498,-30.1107909830603,10.));
#10129=CARTESIAN_POINT('Ctrl Pts',(37.2871105716039,-30.0176605870496,10.));
#10130=CARTESIAN_POINT('Ctrl Pts',(37.2983003551911,-29.9248411115275,10.));
#10131=CARTESIAN_POINT('Ctrl Pts',(37.3140907933662,-29.832721945892,10.));
#10132=CARTESIAN_POINT('Ctrl Pts',(37.3296581165649,-29.7419044012272,10.));
#10133=CARTESIAN_POINT('Ctrl Pts',(37.3496974685084,-29.6517666687559,10.));
#10134=CARTESIAN_POINT('Ctrl Pts',(37.3741667173832,-29.5627070154397,10.));
#10135=CARTESIAN_POINT('Ctrl Pts',(37.3836803734301,-29.5280805782472,10.));
#10136=CARTESIAN_POINT('Ctrl Pts',(37.393864106677,-29.4936174486057,10.));
#10137=CARTESIAN_POINT('Ctrl Pts',(37.4047170075811,-29.4593424965086,10.));
#10138=CARTESIAN_POINT('Ctrl Pts',(37.4105212308036,-29.4410119621504,10.));
#10139=CARTESIAN_POINT('Ctrl Pts',(37.4165168636927,-29.4227352659255,10.));
#10140=CARTESIAN_POINT('Ctrl Pts',(37.4227038628238,-29.4045163264401,10.));
#10141=CARTESIAN_POINT('Ctrl Pts',(37.4281525019749,-29.3884716455105,10.));
#10142=CARTESIAN_POINT('Ctrl Pts',(37.433750036472,-29.3724706840406,10.));
#10143=CARTESIAN_POINT('Ctrl Pts',(37.4394903150468,-29.3565325286955,10.));
#10144=CARTESIAN_POINT('Ctrl Pts',(37.4719158315028,-29.266501546456,10.));
#10145=CARTESIAN_POINT('Ctrl Pts',(37.508932391867,-29.178349298418,10.));
#10146=CARTESIAN_POINT('Ctrl Pts',(37.5504669605507,-29.0925203605859,10.));
#10147=CARTESIAN_POINT('Ctrl Pts',(37.5816178870634,-29.0281486572119,10.));
#10148=CARTESIAN_POINT('Ctrl Pts',(37.6153113416024,-28.9650843527885,10.));
#10149=CARTESIAN_POINT('Ctrl Pts',(37.6515338806021,-28.9035321598138,10.));
#10150=CARTESIAN_POINT('Ctrl Pts',(37.6664656394419,-28.8781589384178,10.));
#10151=CARTESIAN_POINT('Ctrl Pts',(37.6818273228934,-28.8530428664222,10.));
#10152=CARTESIAN_POINT('Ctrl Pts',(37.6976186471279,-28.8281991892111,10.));
#10153=CARTESIAN_POINT('Ctrl Pts',(37.707051317448,-28.8133592547514,10.));
#10154=CARTESIAN_POINT('Ctrl Pts',(37.7166326076961,-28.7986239321154,10.));
#10155=CARTESIAN_POINT('Ctrl Pts',(37.7263604788376,-28.7839985432967,10.));
#10156=CARTESIAN_POINT('Ctrl Pts',(37.7738891331826,-28.7125414855586,10.));
#10157=CARTESIAN_POINT('Ctrl Pts',(37.8249265653207,-28.6436864116098,10.));
#10158=CARTESIAN_POINT('Ctrl Pts',(37.8794383922861,-28.5777860374312,10.));
#10159=CARTESIAN_POINT('Ctrl Pts',(37.9310245147155,-28.5154226025628,10.));
#10160=CARTESIAN_POINT('Ctrl Pts',(37.9857225827401,-28.4557049960579,10.));
#10161=CARTESIAN_POINT('Ctrl Pts',(38.0435272485066,-28.3989680111034,10.));
#10162=CARTESIAN_POINT('Ctrl Pts',(38.0564932251206,-28.3862415225005,10.));
#10163=CARTESIAN_POINT('Ctrl Pts',(38.0696155913077,-28.3736651582161,10.));
#10164=CARTESIAN_POINT('Ctrl Pts',(38.0828911169303,-28.3612402481786,10.));
#10165=CARTESIAN_POINT('Ctrl Pts',(-38.0865340033349,31.635987203375,10.));
#10166=CARTESIAN_POINT('Ctrl Pts',(-38.0249212302155,31.5780863258049,10.));
#10167=CARTESIAN_POINT('Ctrl Pts',(-37.9666796325226,31.517034936212,10.));
#10168=CARTESIAN_POINT('Ctrl Pts',(-37.9118060982863,31.4532178325339,10.));
#10169=CARTESIAN_POINT('Ctrl Pts',(-37.855479884161,31.387711283764,10.));
#10170=CARTESIAN_POINT('Ctrl Pts',(-37.802701985108,31.3192902159922,10.));
#10171=CARTESIAN_POINT('Ctrl Pts',(-37.7534945847852,31.2483222499473,10.));
#10172=CARTESIAN_POINT('Ctrl Pts',(-37.7025929329964,31.1749107981721,10.));
#10173=CARTESIAN_POINT('Ctrl Pts',(-37.6555113004629,31.0987735233447,10.));
#10174=CARTESIAN_POINT('Ctrl Pts',(-37.6123091713429,31.0202733477527,10.));
#10175=CARTESIAN_POINT('Ctrl Pts',(-37.5934082398529,30.9859295209312,10.));
#10176=CARTESIAN_POINT('Ctrl Pts',(-37.5752503635828,30.9511329138551,10.));
#10177=CARTESIAN_POINT('Ctrl Pts',(-37.5578429689868,30.915911828878,10.));
#10178=CARTESIAN_POINT('Ctrl Pts',(-37.5483347565091,30.8966734783134,10.));
#10179=CARTESIAN_POINT('Ctrl Pts',(-37.5390504796292,30.8773084638734,10.));
#10180=CARTESIAN_POINT('Ctrl Pts',(-37.5299915522756,30.8578212692062,10.));
#10181=CARTESIAN_POINT('Ctrl Pts',(-37.5213415858625,30.8392138146172,10.));
#10182=CARTESIAN_POINT('Ctrl Pts',(-37.5128945913309,30.8204889632415,10.));
#10183=CARTESIAN_POINT('Ctrl Pts',(-37.5046658996397,30.801683398448,10.));
#10184=CARTESIAN_POINT('Ctrl Pts',(-37.4681050714562,30.7181285577627,10.));
#10185=CARTESIAN_POINT('Ctrl Pts',(-37.4358044628107,30.6328902559792,10.));
#10186=CARTESIAN_POINT('Ctrl Pts',(-37.4077883457094,30.5463673398094,10.));
#10187=CARTESIAN_POINT('Ctrl Pts',(-37.3793099418999,30.4584167313599,10.));
#10188=CARTESIAN_POINT('Ctrl Pts',(-37.3552580988168,30.3691380088872,10.));
#10189=CARTESIAN_POINT('Ctrl Pts',(-37.3356974176737,30.2789129619801,10.));
#10190=CARTESIAN_POINT('Ctrl Pts',(-37.3164750142936,30.1902482455546,10.));
#10191=CARTESIAN_POINT('Ctrl Pts',(-37.3015895191302,30.1006687433848,10.));
#10192=CARTESIAN_POINT('Ctrl Pts',(-37.2911449398656,30.0105139328834,10.));
#10193=CARTESIAN_POINT('Ctrl Pts',(-37.287014788403,29.9748635717711,10.));
#10194=CARTESIAN_POINT('Ctrl Pts',(-37.2835795539213,29.9391230694737,10.));
#10195=CARTESIAN_POINT('Ctrl Pts',(-37.2808476966539,29.9033128824872,10.));
#10196=CARTESIAN_POINT('Ctrl Pts',(-37.2792307868413,29.8821178356521,10.));
#10197=CARTESIAN_POINT('Ctrl Pts',(-37.2778603014039,29.8608983733072,10.));
#10198=CARTESIAN_POINT('Ctrl Pts',(-37.2767381968828,29.8396587140598,10.));
#10199=CARTESIAN_POINT('Ctrl Pts',(-37.2759912880507,29.825520914251,10.));
#10200=CARTESIAN_POINT('Ctrl Pts',(-37.2753545077548,29.8113741694225,10.));
#10201=CARTESIAN_POINT('Ctrl Pts',(-37.2748287840665,29.79723427985,10.));
#10202=CARTESIAN_POINT('Ctrl Pts',(-37.2712900173062,29.7020554390877,10.));
#10203=CARTESIAN_POINT('Ctrl Pts',(-37.2727699852428,29.6070256281828,10.));
#10204=CARTESIAN_POINT('Ctrl Pts',(-37.2793273367095,29.5125435687522,10.));
#10205=CARTESIAN_POINT('Ctrl Pts',(-37.2858621977529,29.418385564165,10.));
#10206=CARTESIAN_POINT('Ctrl Pts',(-37.2974393139327,29.3247706066949,10.));
#10207=CARTESIAN_POINT('Ctrl Pts',(-37.3141647303328,29.2320754265285,10.));
#10208=CARTESIAN_POINT('Ctrl Pts',(-37.3161015946175,29.2213409862291,10.));
#10209=CARTESIAN_POINT('Ctrl Pts',(-37.3181075567504,29.2106188701492,10.));
#10210=CARTESIAN_POINT('Ctrl Pts',(-37.3201828266509,29.1999096568791,10.));
#10211=CARTESIAN_POINT('Ctrl Pts',(-37.33772774812,29.1093709246518,10.));
#10212=CARTESIAN_POINT('Ctrl Pts',(-37.360222053948,29.0197541127662,10.));
#10213=CARTESIAN_POINT('Ctrl Pts',(-37.3873904512652,28.9312971488731,10.));
#10214=CARTESIAN_POINT('Ctrl Pts',(-37.3981387282381,28.8963020795282,10.));
#10215=CARTESIAN_POINT('Ctrl Pts',(-37.4096191399982,28.8614885919146,10.));
#10216=CARTESIAN_POINT('Ctrl Pts',(-37.4218168347016,28.826871760633,10.));
#10217=CARTESIAN_POINT('Ctrl Pts',(-37.4277710430044,28.8099738279297,10.));
#10218=CARTESIAN_POINT('Ctrl Pts',(-37.4338961854739,28.7931227592818,10.));
#10219=CARTESIAN_POINT('Ctrl Pts',(-37.4401906356363,28.7763203362452,10.));
#10220=CARTESIAN_POINT('Ctrl Pts',(-37.4454353749813,28.7623200142288,10.));
#10221=CARTESIAN_POINT('Ctrl Pts',(-37.4507947656063,28.7483612736679,10.));
#10222=CARTESIAN_POINT('Ctrl Pts',(-37.4562655924271,28.7344496968282,10.));
#10223=CARTESIAN_POINT('Ctrl Pts',(-37.4904901961104,28.6474211324931,10.));
#10224=CARTESIAN_POINT('Ctrl Pts',(-37.5290932417427,28.5621806872409,10.));
#10225=CARTESIAN_POINT('Ctrl Pts',(-37.5717422429702,28.4789602337942,10.));
#10226=CARTESIAN_POINT('Ctrl Pts',(-37.6159714723182,28.3926563013224,10.));
#10227=CARTESIAN_POINT('Ctrl Pts',(-37.6645521622043,28.3085240970534,10.));
#10228=CARTESIAN_POINT('Ctrl Pts',(-37.7171694435466,28.2268257622467,10.));
#10229=CARTESIAN_POINT('Ctrl Pts',(-37.770364364078,28.1442305327571,10.));
#10230=CARTESIAN_POINT('Ctrl Pts',(-37.8276854092032,28.0641220869244,10.));
#10231=CARTESIAN_POINT('Ctrl Pts',(-37.8888588427698,27.9867866516892,10.));
#10232=CARTESIAN_POINT('Ctrl Pts',(-37.9126758941047,27.9566771429758,10.));
#10233=CARTESIAN_POINT('Ctrl Pts',(-37.9370774163132,27.9269882051562,10.));
#10234=CARTESIAN_POINT('Ctrl Pts',(-37.9620491203782,27.8977377702384,10.));
#10235=CARTESIAN_POINT('Ctrl Pts',(-37.982034894532,27.8743275702518,10.));
#10236=CARTESIAN_POINT('Ctrl Pts',(-38.0023859127899,27.8511982591558,10.));
#10237=CARTESIAN_POINT('Ctrl Pts',(-38.0230952862197,27.8283593716466,10.));
#10238=CARTESIAN_POINT('Ctrl Pts',(-38.0346445261292,27.8156225405686,10.));
#10239=CARTESIAN_POINT('Ctrl Pts',(-38.0463001486068,27.8029816946559,10.));
#10240=CARTESIAN_POINT('Ctrl Pts',(-38.0580558973667,27.7904432603858,10.));
#10241=CARTESIAN_POINT('Ctrl Pts',(-38.1271112801678,27.716790242111,10.));
#10242=CARTESIAN_POINT('Ctrl Pts',(-38.1996672523087,27.6466146571222,10.));
#10243=CARTESIAN_POINT('Ctrl Pts',(-38.2754118739757,27.5802053578348,10.));
#10244=CARTESIAN_POINT('Ctrl Pts',(-38.3396628308816,27.5238731598152,10.));
#10245=CARTESIAN_POINT('Ctrl Pts',(-38.4062092138265,27.470250936803,10.));
#10246=CARTESIAN_POINT('Ctrl Pts',(-38.4748854868873,27.419529916892,10.));
#10247=CARTESIAN_POINT('Ctrl Pts',(-38.4975744224142,27.4027729512132,10.));
#10248=CARTESIAN_POINT('Ctrl Pts',(-38.5204959977952,27.3863327822983,10.));
#10249=CARTESIAN_POINT('Ctrl Pts',(-38.5436447147886,27.3702167463987,10.));
#10250=CARTESIAN_POINT('Ctrl Pts',(-38.5602398136962,27.3586633108528,10.));
#10251=CARTESIAN_POINT('Ctrl Pts',(-38.5769526172639,27.3472759337365,10.));
#10252=CARTESIAN_POINT('Ctrl Pts',(-38.5937665384207,27.3360668068749,10.));
#10253=CARTESIAN_POINT('Ctrl Pts',(-38.6801204221607,27.2784983415061,10.));
#10254=CARTESIAN_POINT('Ctrl Pts',(-38.7692236972918,27.2255681352496,10.));
#10255=CARTESIAN_POINT('Ctrl Pts',(-38.8607678183074,27.1775976530154,10.));
#10256=CARTESIAN_POINT('Ctrl Pts',(-38.952311939323,27.1296271707811,10.));
#10257=CARTESIAN_POINT('Ctrl Pts',(-39.0462975515555,27.0866155018757,10.));
#10258=CARTESIAN_POINT('Ctrl Pts',(-39.1424541530616,27.0489248578152,10.));
#10259=CARTESIAN_POINT('Ctrl Pts',(-39.1630221217565,27.0408628009727,10.));
#10260=CARTESIAN_POINT('Ctrl Pts',(-39.1836895389297,27.0330443769238,10.));
#10261=CARTESIAN_POINT('Ctrl Pts',(-39.2044525003272,27.0254684088901,10.));
#10262=CARTESIAN_POINT('Ctrl Pts',(-40.7937992825329,27.0307770462543,10.));
#10263=CARTESIAN_POINT('Ctrl Pts',(-40.8868534224289,27.0648166662984,10.));
#10264=CARTESIAN_POINT('Ctrl Pts',(-40.9778403384339,27.1036257277316,10.));
#10265=CARTESIAN_POINT('Ctrl Pts',(-41.0665522485249,27.1468755032666,10.));
#10266=CARTESIAN_POINT('Ctrl Pts',(-41.1572339280192,27.1910856017668,10.));
#10267=CARTESIAN_POINT('Ctrl Pts',(-41.2455391179634,27.2399364251585,10.));
#10268=CARTESIAN_POINT('Ctrl Pts',(-41.3312169493438,27.2931224121673,10.));
#10269=CARTESIAN_POINT('Ctrl Pts',(-41.414166339304,27.3446146722506,10.));
#10270=CARTESIAN_POINT('Ctrl Pts',(-41.4946533698995,27.4001712453837,10.));
#10271=CARTESIAN_POINT('Ctrl Pts',(-41.5724166737304,27.459545531637,10.));
#10272=CARTESIAN_POINT('Ctrl Pts',(-41.6404595645825,27.5114980321086,10.));
#10273=CARTESIAN_POINT('Ctrl Pts',(-41.7064168053658,27.5663741861413,10.));
#10274=CARTESIAN_POINT('Ctrl Pts',(-41.7700880360598,27.6240217668293,10.));
#10275=CARTESIAN_POINT('Ctrl Pts',(-41.7834305900767,27.6361020415607,10.));
#10276=CARTESIAN_POINT('Ctrl Pts',(-41.7966745289852,27.6483059196791,10.));
#10277=CARTESIAN_POINT('Ctrl Pts',(-41.8098008297905,27.6606156964746,10.));
#10278=CARTESIAN_POINT('Ctrl Pts',(-41.8822284325512,27.7285379265867,10.));
#10279=CARTESIAN_POINT('Ctrl Pts',(-41.9511903175657,27.7997813678814,10.));
#10280=CARTESIAN_POINT('Ctrl Pts',(-42.0164471409414,27.8740548505011,10.));
#10281=CARTESIAN_POINT('Ctrl Pts',(-42.0813426208374,27.947917062126,10.));
#10282=CARTESIAN_POINT('Ctrl Pts',(-42.1425744423444,28.0247766498528,10.));
#10283=CARTESIAN_POINT('Ctrl Pts',(-42.1998636016162,28.1043739992373,10.));
#10284=CARTESIAN_POINT('Ctrl Pts',(-42.2557187057104,28.1819788775774,10.));
#10285=CARTESIAN_POINT('Ctrl Pts',(-42.3078263315155,28.2621869103881,10.));
#10286=CARTESIAN_POINT('Ctrl Pts',(-42.3558810447646,28.3447716158106,10.));
#10287=CARTESIAN_POINT('Ctrl Pts',(-42.3766086283242,28.3803931244337,10.));
#10288=CARTESIAN_POINT('Ctrl Pts',(-42.3965815502584,28.4164569256333,10.));
#10289=CARTESIAN_POINT('Ctrl Pts',(-42.4157723168559,28.4529451771185,10.));
#10290=CARTESIAN_POINT('Ctrl Pts',(-42.4294376380156,28.4789276553363,10.));
#10291=CARTESIAN_POINT('Ctrl Pts',(-42.4427063253691,28.5051253564734,10.));
#10292=CARTESIAN_POINT('Ctrl Pts',(-42.4555678554338,28.5315318420532,10.));
#10293=CARTESIAN_POINT('Ctrl Pts',(-42.4611833404534,28.5430612031361,10.));
#10294=CARTESIAN_POINT('Ctrl Pts',(-42.4667202817154,28.554628567478,10.));
#10295=CARTESIAN_POINT('Ctrl Pts',(-42.4721741089808,28.5662251224027,10.));
#10296=CARTESIAN_POINT('Ctrl Pts',(-42.512401961449,28.6517622100199,10.));
#10297=CARTESIAN_POINT('Ctrl Pts',(-42.54817377646,28.7390124376936,10.));
#10298=CARTESIAN_POINT('Ctrl Pts',(-42.5792385749088,28.8277384868494,10.));
#10299=CARTESIAN_POINT('Ctrl Pts',(-42.6096166633377,28.9145031819959,10.));
#10300=CARTESIAN_POINT('Ctrl Pts',(-42.6354937565339,29.0026798461803,10.));
#10301=CARTESIAN_POINT('Ctrl Pts',(-42.6565860361294,29.0920553698958,10.));
#10302=CARTESIAN_POINT('Ctrl Pts',(-42.6603147481206,29.1078552546589,10.));
#10303=CARTESIAN_POINT('Ctrl Pts',(-42.6638937963736,29.1236926137693,10.));
#10304=CARTESIAN_POINT('Ctrl Pts',(-42.6673214406689,29.1395662754716,10.));
#10305=CARTESIAN_POINT('Ctrl Pts',(-42.6874323400132,29.232701264176,10.));
#10306=CARTESIAN_POINT('Ctrl Pts',(-42.7023352690137,29.3270870046807,10.));
#10307=CARTESIAN_POINT('Ctrl Pts',(-42.7121087193039,29.4223145987471,10.));
#10308=CARTESIAN_POINT('Ctrl Pts',(-42.7153866067918,29.4542526891688,10.));
#10309=CARTESIAN_POINT('Ctrl Pts',(-42.7180870912415,29.4862853537632,10.));
#10310=CARTESIAN_POINT('Ctrl Pts',(-42.7202119090113,29.5183966971079,10.));
#10311=CARTESIAN_POINT('Ctrl Pts',(-42.7214005292254,29.5363597395597,10.));
#10312=CARTESIAN_POINT('Ctrl Pts',(-42.7224089972278,29.5543473974331,10.));
#10313=CARTESIAN_POINT('Ctrl Pts',(-42.7232375376159,29.5723568432295,10.));
#10314=CARTESIAN_POINT('Ctrl Pts',(-42.7238118031779,29.5848392818196,10.));
#10315=CARTESIAN_POINT('Ctrl Pts',(-42.7242995172634,29.5973306577781,10.));
#10316=CARTESIAN_POINT('Ctrl Pts',(-42.7247006297286,29.609820549451,10.));
#10317=CARTESIAN_POINT('Ctrl Pts',(-42.7276934506505,29.7030113932964,10.));
#10318=CARTESIAN_POINT('Ctrl Pts',(-42.7258766829749,29.7962666945407,10.));
#10319=CARTESIAN_POINT('Ctrl Pts',(-42.7193894300159,29.8892113227638,10.));
#10320=CARTESIAN_POINT('Ctrl Pts',(-42.7128892185463,29.9823416110736,10.));
#10321=CARTESIAN_POINT('Ctrl Pts',(-42.701699460792,30.0751609655971,10.));
#10322=CARTESIAN_POINT('Ctrl Pts',(-42.6859090498045,30.1672800015875,10.));
#10323=CARTESIAN_POINT('Ctrl Pts',(-42.6703417487034,30.2580974458921,10.));
#10324=CARTESIAN_POINT('Ctrl Pts',(-42.6503024174743,30.3482350691811,10.));
#10325=CARTESIAN_POINT('Ctrl Pts',(-42.6258331870985,30.4372946086112,10.));
#10326=CARTESIAN_POINT('Ctrl Pts',(-42.6163195250727,30.4719210494636,10.));
#10327=CARTESIAN_POINT('Ctrl Pts',(-42.606135783656,30.5063841816026,10.));
#10328=CARTESIAN_POINT('Ctrl Pts',(-42.5952828723427,30.5406591351763,10.));
#10329=CARTESIAN_POINT('Ctrl Pts',(-42.5894786544185,30.5589896360104,10.));
#10330=CARTESIAN_POINT('Ctrl Pts',(-42.5834830269037,30.5772662986208,10.));
#10331=CARTESIAN_POINT('Ctrl Pts',(-42.5772960332143,30.5954852044445,10.));
#10332=CARTESIAN_POINT('Ctrl Pts',(-42.5718474280992,30.6115297696157,10.));
#10333=CARTESIAN_POINT('Ctrl Pts',(-42.5662499293154,30.6275306156841,10.));
#10334=CARTESIAN_POINT('Ctrl Pts',(-42.5605096880314,30.6434686563279,10.));
#10335=CARTESIAN_POINT('Ctrl Pts',(-42.5280842026754,30.7334994891673,10.));
#10336=CARTESIAN_POINT('Ctrl Pts',(-42.4910676731712,30.8216515881688,10.));
#10337=CARTESIAN_POINT('Ctrl Pts',(-42.4495331341105,30.9074803825421,10.));
#10338=CARTESIAN_POINT('Ctrl Pts',(-42.418382229815,30.9718519783221,10.));
#10339=CARTESIAN_POINT('Ctrl Pts',(-42.3846887967975,31.0349161782887,10.));
#10340=CARTESIAN_POINT('Ctrl Pts',(-42.3484662781896,31.0964682722131,10.));
#10341=CARTESIAN_POINT('Ctrl Pts',(-42.3335345030887,31.1218414946943,10.));
#10342=CARTESIAN_POINT('Ctrl Pts',(-42.3181728017638,31.1469575678454,10.));
#10343=CARTESIAN_POINT('Ctrl Pts',(-42.3023814580131,31.1718012463697,10.));
#10344=CARTESIAN_POINT('Ctrl Pts',(-42.2929488091092,31.1866411295805,10.));
#10345=CARTESIAN_POINT('Ctrl Pts',(-42.2833675408082,31.2013764016503,9.99999999999999));
#10346=CARTESIAN_POINT('Ctrl Pts',(-42.2736396920405,31.2160017407882,9.99999999999999));
#10347=CARTESIAN_POINT('Ctrl Pts',(-42.2261110200766,31.2874587466322,9.99999999999999));
#10348=CARTESIAN_POINT('Ctrl Pts',(-42.1750735624793,31.3563137747452,10.));
#10349=CARTESIAN_POINT('Ctrl Pts',(-42.1205617015116,31.4222141122843,10.));
#10350=CARTESIAN_POINT('Ctrl Pts',(-42.0689756436836,31.4845773954821,10.));
#10351=CARTESIAN_POINT('Ctrl Pts',(-42.0142776442785,31.5442948684644,9.99999999999999));
#10352=CARTESIAN_POINT('Ctrl Pts',(-41.9564730504323,31.6010317426951,9.99999999999999));
#10353=CARTESIAN_POINT('Ctrl Pts',(-41.9435070760097,31.6137582201452,9.99999999999999));
#10354=CARTESIAN_POINT('Ctrl Pts',(-41.9303847118439,31.6263345741028,9.99999999999999));
#10355=CARTESIAN_POINT('Ctrl Pts',(-41.9171091880767,31.6387594746126,9.99999999999999));
#10356=CARTESIAN_POINT('Ctrl Pts',(41.9134659966651,31.6359872033749,10.));
#10357=CARTESIAN_POINT('Ctrl Pts',(41.9750786368702,31.5780864507117,10.));
#10358=CARTESIAN_POINT('Ctrl Pts',(42.0333200948858,31.5170351770757,10.));
#10359=CARTESIAN_POINT('Ctrl Pts',(42.0881934870624,31.4532181824915,10.));
#10360=CARTESIAN_POINT('Ctrl Pts',(42.1445195700427,31.3877117286362,10.));
#10361=CARTESIAN_POINT('Ctrl Pts',(42.1972973335829,31.3192907470308,10.));
#10362=CARTESIAN_POINT('Ctrl Pts',(42.2465045986483,31.2483228609998,10.));
#10363=CARTESIAN_POINT('Ctrl Pts',(42.2974062316616,31.1749113172842,10.));
#10364=CARTESIAN_POINT('Ctrl Pts',(42.344487827514,31.0987739309724,10.));
#10365=CARTESIAN_POINT('Ctrl Pts',(42.3876899067312,31.0202736297946,10.));
#10366=CARTESIAN_POINT('Ctrl Pts',(42.4065908163888,30.9859297480294,10.));
#10367=CARTESIAN_POINT('Ctrl Pts',(42.4247486682925,30.951133083306,10.));
#10368=CARTESIAN_POINT('Ctrl Pts',(42.4421560363682,30.9159119384179,10.));
#10369=CARTESIAN_POINT('Ctrl Pts',(42.4516643000981,30.8966734221178,10.));
#10370=CARTESIAN_POINT('Ctrl Pts',(42.4609486244912,30.8773082395153,10.));
#10371=CARTESIAN_POINT('Ctrl Pts',(42.4700075956502,30.8578208744221,10.));
#10372=CARTESIAN_POINT('Ctrl Pts',(42.4786576094824,30.8392132450731,10.));
#10373=CARTESIAN_POINT('Ctrl Pts',(42.4871046478346,30.8204882165881,10.));
#10374=CARTESIAN_POINT('Ctrl Pts',(42.4953333795948,30.8016824730484,10.));
#10375=CARTESIAN_POINT('Ctrl Pts',(42.5318940411399,30.7181276258749,10.));
#10376=CARTESIAN_POINT('Ctrl Pts',(42.5641944897046,30.6328893164368,10.));
#10377=CARTESIAN_POINT('Ctrl Pts',(42.5922104581374,30.5463663947005,10.));
#10378=CARTESIAN_POINT('Ctrl Pts',(42.6206887314238,30.458415716977,10.));
#10379=CARTESIAN_POINT('Ctrl Pts',(42.6447404493657,30.3691369254667,10.));
#10380=CARTESIAN_POINT('Ctrl Pts',(42.6643010157385,30.2789118139978,10.));
#10381=CARTESIAN_POINT('Ctrl Pts',(42.6835233268679,30.1902469394079,10.));
#10382=CARTESIAN_POINT('Ctrl Pts',(42.698408730528,30.1006672814378,10.));
#10383=CARTESIAN_POINT('Ctrl Pts',(42.7088532234977,30.0105123225977,10.));
#10384=CARTESIAN_POINT('Ctrl Pts',(42.7129833484531,29.9748618370792,10.));
#10385=CARTESIAN_POINT('Ctrl Pts',(42.7164185546788,29.9391212112098,10.));
#10386=CARTESIAN_POINT('Ctrl Pts',(42.7191503821694,29.9033109019147,10.));
#10387=CARTESIAN_POINT('Ctrl Pts',(42.7207672703654,29.8821158350244,10.));
#10388=CARTESIAN_POINT('Ctrl Pts',(42.7221377348703,29.8608963531876,10.));
#10389=CARTESIAN_POINT('Ctrl Pts',(42.7232598192034,29.8396566750697,10.));
#10390=CARTESIAN_POINT('Ctrl Pts',(42.7240067154734,29.8255188461256,10.));
#10391=CARTESIAN_POINT('Ctrl Pts',(42.7246434832814,29.8113720723697,10.));
#10392=CARTESIAN_POINT('Ctrl Pts',(42.7251691945808,29.7972321541886,10.));
#10393=CARTESIAN_POINT('Ctrl Pts',(42.7287078734581,29.7020532416424,10.));
#10394=CARTESIAN_POINT('Ctrl Pts',(42.7272278347504,29.6070233725301,10.));
#10395=CARTESIAN_POINT('Ctrl Pts',(42.7206704346253,29.5125412731866,10.));
#10396=CARTESIAN_POINT('Ctrl Pts',(42.7141355191106,29.4183831426661,10.));
#10397=CARTESIAN_POINT('Ctrl Pts',(42.7025583611906,29.3247680784185,10.));
#10398=CARTESIAN_POINT('Ctrl Pts',(42.6858329205046,29.2320728163631,10.));
#10399=CARTESIAN_POINT('Ctrl Pts',(42.6838960555975,29.2213383787185,10.));
#10400=CARTESIAN_POINT('Ctrl Pts',(42.6818900932326,29.2106162655995,10.));
#10401=CARTESIAN_POINT('Ctrl Pts',(42.6798148234985,29.1999070556032,10.));
#10402=CARTESIAN_POINT('Ctrl Pts',(42.6622698775574,29.1093682175089,10.));
#10403=CARTESIAN_POINT('Ctrl Pts',(42.6397755611135,29.0197513248276,10.));
#10404=CARTESIAN_POINT('Ctrl Pts',(42.6126071639148,28.931294302045,10.));
#10405=CARTESIAN_POINT('Ctrl Pts',(42.6018588686328,28.8962991496375,10.));
#10406=CARTESIAN_POINT('Ctrl Pts',(42.5903784377438,28.861485583013,10.));
#10407=CARTESIAN_POINT('Ctrl Pts',(42.5781807229744,28.8268686766644,10.));
#10408=CARTESIAN_POINT('Ctrl Pts',(42.5722259508754,28.8099691350719,10.));
#10409=CARTESIAN_POINT('Ctrl Pts',(42.5661002125772,28.7931164671958,10.));
#10410=CARTESIAN_POINT('Ctrl Pts',(42.5598051349902,28.7763124550784,10.));
#10411=CARTESIAN_POINT('Ctrl Pts',(42.5545609327821,28.7623136383469,10.));
#10412=CARTESIAN_POINT('Ctrl Pts',(42.5492021060364,28.7483563994138,10.));
#10413=CARTESIAN_POINT('Ctrl Pts',(42.543731866508,28.7344463125978,10.));
#10414=CARTESIAN_POINT('Ctrl Pts',(42.5095072459392,28.6474176841639,10.));
#10415=CARTESIAN_POINT('Ctrl Pts',(42.4709041883668,28.5621771974268,10.));
#10416=CARTESIAN_POINT('Ctrl Pts',(42.4282551773101,28.4789567220783,10.));
#10417=CARTESIAN_POINT('Ctrl Pts',(42.384025973209,28.3926528360469,10.));
#10418=CARTESIAN_POINT('Ctrl Pts',(42.33544531781,28.3085206957999,10.));
#10419=CARTESIAN_POINT('Ctrl Pts',(42.2828280762731,28.2268224389197,10.));
#10420=CARTESIAN_POINT('Ctrl Pts',(42.2296332219524,28.144227328533,10.));
#10421=CARTESIAN_POINT('Ctrl Pts',(42.172312252504,28.0641190135926,10.));
#10422=CARTESIAN_POINT('Ctrl Pts',(42.111138899714,27.9867837170881,10.));
#10423=CARTESIAN_POINT('Ctrl Pts',(42.0873215657202,27.9566738652924,10.));
#10424=CARTESIAN_POINT('Ctrl Pts',(42.0629197462126,27.9269845966725,10.));
#10425=CARTESIAN_POINT('Ctrl Pts',(42.0379477305135,27.8977338437241,10.));
#10426=CARTESIAN_POINT('Ctrl Pts',(42.0179551026749,27.8743156533487,10.));
#10427=CARTESIAN_POINT('Ctrl Pts',(41.9975969801375,27.8511785456982,10.));
#10428=CARTESIAN_POINT('Ctrl Pts',(41.9768802587376,27.8283320652486,10.));
#10429=CARTESIAN_POINT('Ctrl Pts',(41.9653377723937,27.8156029666857,10.));
#10430=CARTESIAN_POINT('Ctrl Pts',(41.9536890484812,27.802969758936,10.));
#10431=CARTESIAN_POINT('Ctrl Pts',(41.9419403107313,27.7904388332169,10.));
#10432=CARTESIAN_POINT('Ctrl Pts',(41.8728849423382,27.7167860110788,10.));
#10433=CARTESIAN_POINT('Ctrl Pts',(41.8003289871598,27.6466106302074,10.));
#10434=CARTESIAN_POINT('Ctrl Pts',(41.7245843802806,27.580201539271,10.));
#10435=CARTESIAN_POINT('Ctrl Pts',(41.6603337326078,27.5238697781091,10.));
#10436=CARTESIAN_POINT('Ctrl Pts',(41.5937876785201,27.4702479699947,10.));
#10437=CARTESIAN_POINT('Ctrl Pts',(41.5251117488698,27.419527338206,10.));
#10438=CARTESIAN_POINT('Ctrl Pts',(41.5024197920256,27.4027681855666,10.));
#10439=CARTESIAN_POINT('Ctrl Pts',(41.4794951326352,27.3863259143062,10.));
#10440=CARTESIAN_POINT('Ctrl Pts',(41.4563432710306,27.3702078635546,10.));
#10441=CARTESIAN_POINT('Ctrl Pts',(41.439752008952,27.3586572241813,10.));
#10442=CARTESIAN_POINT('Ctrl Pts',(41.4230430998386,27.3472725679575,10.));
#10443=CARTESIAN_POINT('Ctrl Pts',(41.4062331203527,27.3360660788018,10.));
#10444=CARTESIAN_POINT('Ctrl Pts',(41.3198794116228,27.278497781277,10.));
#10445=CARTESIAN_POINT('Ctrl Pts',(41.2307763052375,27.2255677270881,10.));
#10446=CARTESIAN_POINT('Ctrl Pts',(41.1392323413556,27.177597375897,10.));
#10447=CARTESIAN_POINT('Ctrl Pts',(41.0476883774738,27.1296270247058,10.));
#10448=CARTESIAN_POINT('Ctrl Pts',(40.9537029107743,27.0866154658313,10.));
#10449=CARTESIAN_POINT('Ctrl Pts',(40.8575464379022,27.0489249053832,10.));
#10450=CARTESIAN_POINT('Ctrl Pts',(40.8369784825986,27.0408628608893,10.));
#10451=CARTESIAN_POINT('Ctrl Pts',(40.8163110779066,27.0330444483139,10.));
#10452=CARTESIAN_POINT('Ctrl Pts',(40.7955481281091,27.0254684909089,10.));
#10453=CARTESIAN_POINT('Ctrl Pts',(39.2062007174671,27.0307770462543,10.));
#10454=CARTESIAN_POINT('Ctrl Pts',(39.1131465233113,27.0648166861469,10.));
#10455=CARTESIAN_POINT('Ctrl Pts',(39.0221595534034,27.1036257598841,10.));
#10456=CARTESIAN_POINT('Ctrl Pts',(38.9334475905781,27.1468755422436,10.));
#10457=CARTESIAN_POINT('Ctrl Pts',(38.8427658845523,27.1910856343743,10.));
#10458=CARTESIAN_POINT('Ctrl Pts',(38.754460667862,27.2399364428682,10.));
#10459=CARTESIAN_POINT('Ctrl Pts',(38.6687828102117,27.2931224089196,10.));
#10460=CARTESIAN_POINT('Ctrl Pts',(38.5858334272673,27.3446146285694,10.));
#10461=CARTESIAN_POINT('Ctrl Pts',(38.5053464022086,27.4001711524073,10.));
#10462=CARTESIAN_POINT('Ctrl Pts',(38.427583102789,27.4595453830244,10.));
#10463=CARTESIAN_POINT('Ctrl Pts',(38.3595402157968,27.5114978348144,10.));
#10464=CARTESIAN_POINT('Ctrl Pts',(38.2935829780114,27.5663739353082,10.));
#10465=CARTESIAN_POINT('Ctrl Pts',(38.229911749687,27.6240214592988,10.));
#10466=CARTESIAN_POINT('Ctrl Pts',(38.2165692334771,27.6361016883684,10.));
#10467=CARTESIAN_POINT('Ctrl Pts',(38.2033253318375,27.6483055199554,10.));
#10468=CARTESIAN_POINT('Ctrl Pts',(38.1901990676262,27.6606152495089,10.));
#10469=CARTESIAN_POINT('Ctrl Pts',(38.1177714560464,27.7285374165783,10.));
#10470=CARTESIAN_POINT('Ctrl Pts',(38.0488095620059,27.7997807923481,10.));
#10471=CARTESIAN_POINT('Ctrl Pts',(37.983552729848,27.8740542095836,10.));
#10472=CARTESIAN_POINT('Ctrl Pts',(37.9186572520394,27.9479163438703,10.));
#10473=CARTESIAN_POINT('Ctrl Pts',(37.8574254316395,28.0247758533942,10.));
#10474=CARTESIAN_POINT('Ctrl Pts',(37.8001362727997,28.1043731264343,10.));
#10475=CARTESIAN_POINT('Ctrl Pts',(37.7442811597055,28.181977943431,10.));
#10476=CARTESIAN_POINT('Ctrl Pts',(37.6921735255212,28.2621859175384,10.));
#10477=CARTESIAN_POINT('Ctrl Pts',(37.6441188049395,28.3447705693782,10.));
#10478=CARTESIAN_POINT('Ctrl Pts',(37.6233912222305,28.3803920479923,10.));
#10479=CARTESIAN_POINT('Ctrl Pts',(37.6034183010496,28.4164558199656,10.));
#10480=CARTESIAN_POINT('Ctrl Pts',(37.5842275351277,28.4529440432242,10.));
#10481=CARTESIAN_POINT('Ctrl Pts',(37.5705622652714,28.4789264047118,10.));
#10482=CARTESIAN_POINT('Ctrl Pts',(37.557293626232,28.505123988025,10.));
#10483=CARTESIAN_POINT('Ctrl Pts',(37.5444321413805,28.5315303548389,10.));
#10484=CARTESIAN_POINT('Ctrl Pts',(37.5388166779207,28.5430596603322,10.));
#10485=CARTESIAN_POINT('Ctrl Pts',(37.5332797574667,28.5546269691094,10.));
#10486=CARTESIAN_POINT('Ctrl Pts',(37.5278259503489,28.5662234683187,10.));
#10487=CARTESIAN_POINT('Ctrl Pts',(37.4875980830446,28.6517604925136,10.));
#10488=CARTESIAN_POINT('Ctrl Pts',(37.4518262526605,28.7390106640601,10.));
#10489=CARTESIAN_POINT('Ctrl Pts',(37.4207614384841,28.8277366668812,10.));
#10490=CARTESIAN_POINT('Ctrl Pts',(37.3903833336519,28.9145013196402,10.));
#10491=CARTESIAN_POINT('Ctrl Pts',(37.3645062240159,29.0026779508926,10.));
#10492=CARTESIAN_POINT('Ctrl Pts',(37.3434139281184,29.092053453568,10.));
#10493=CARTESIAN_POINT('Ctrl Pts',(37.3396851656113,29.1078535364538,10.));
#10494=CARTESIAN_POINT('Ctrl Pts',(37.3361060706703,29.1236910950166,10.));
#10495=CARTESIAN_POINT('Ctrl Pts',(37.3326783835832,29.1395649574699,10.));
#10496=CARTESIAN_POINT('Ctrl Pts',(37.3125674868137,29.2326999493804,10.));
#10497=CARTESIAN_POINT('Ctrl Pts',(37.2976645630368,29.3270857062678,10.));
#10498=CARTESIAN_POINT('Ctrl Pts',(37.2878911201781,29.4223133275768,10.));
#10499=CARTESIAN_POINT('Ctrl Pts',(37.2846132361742,29.4542514174737,10.));
#10500=CARTESIAN_POINT('Ctrl Pts',(37.2819127551077,29.4862840827079,10.));
#10501=CARTESIAN_POINT('Ctrl Pts',(37.2797879406052,29.5183954277846,10.));
#10502=CARTESIAN_POINT('Ctrl Pts',(37.2785993218355,29.5363584769983,10.));
#10503=CARTESIAN_POINT('Ctrl Pts',(37.2775908553575,29.5543461419914,10.));
#10504=CARTESIAN_POINT('Ctrl Pts',(37.2767623165709,29.5723555952498,10.));
#10505=CARTESIAN_POINT('Ctrl Pts',(37.2761880522997,29.584838035077,10.));
#10506=CARTESIAN_POINT('Ctrl Pts',(37.2757003394872,29.5973294124411,10.));
#10507=CARTESIAN_POINT('Ctrl Pts',(37.2752992282755,29.6098193056725,10.));
#10508=CARTESIAN_POINT('Ctrl Pts',(37.2723064158566,29.7030101876157,10.));
#10509=CARTESIAN_POINT('Ctrl Pts',(37.2741231937037,29.7962655355841,10.));
#10510=CARTESIAN_POINT('Ctrl Pts',(37.2806104580608,29.889210216868,10.));
#10511=CARTESIAN_POINT('Ctrl Pts',(37.2871106808443,29.9823405568134,10.));
#10512=CARTESIAN_POINT('Ctrl Pts',(37.2983004509909,30.0751599693494,10.));
#10513=CARTESIAN_POINT('Ctrl Pts',(37.3140908750205,30.1672790674991,10.));
#10514=CARTESIAN_POINT('Ctrl Pts',(37.3296581867233,30.258096559923,10.));
#10515=CARTESIAN_POINT('Ctrl Pts',(37.3496975278913,30.3482342355622,10.));
#10516=CARTESIAN_POINT('Ctrl Pts',(37.3741667671441,30.4372938295988,10.));
#10517=CARTESIAN_POINT('Ctrl Pts',(37.3836804263222,30.4719202687557,10.));
#10518=CARTESIAN_POINT('Ctrl Pts',(37.3938641638431,30.5063833997562,10.));
#10519=CARTESIAN_POINT('Ctrl Pts',(37.4047170701892,30.5406583526803,10.));
#10520=CARTESIAN_POINT('Ctrl Pts',(37.4105212906447,30.5589888695513,10.));
#10521=CARTESIAN_POINT('Ctrl Pts',(37.4165169207267,30.5772655482422,10.));
#10522=CARTESIAN_POINT('Ctrl Pts',(37.4227039170148,30.5954844701692,10.));
#10523=CARTESIAN_POINT('Ctrl Pts',(37.4281525384222,30.6115290907587,10.));
#10524=CARTESIAN_POINT('Ctrl Pts',(37.4337500543009,30.6275299920748,10.));
#10525=CARTESIAN_POINT('Ctrl Pts',(37.4394903134347,30.6434680876312,10.));
#10526=CARTESIAN_POINT('Ctrl Pts',(37.4719158137031,30.7334989921067,10.));
#10527=CARTESIAN_POINT('Ctrl Pts',(37.5089323580049,30.8216511625714,10.));
#10528=CARTESIAN_POINT('Ctrl Pts',(37.5504669112701,30.9074800257348,10.));
#10529=CARTESIAN_POINT('Ctrl Pts',(37.5816178262191,30.9718516731074,10.));
#10530=CARTESIAN_POINT('Ctrl Pts',(37.6153112695565,31.0349159231632,10.));
#10531=CARTESIAN_POINT('Ctrl Pts',(37.6515337979429,31.0964680645853,10.));
#10532=CARTESIAN_POINT('Ctrl Pts',(37.6664655652351,31.1218412865275,10.));
#10533=CARTESIAN_POINT('Ctrl Pts',(37.6818272579777,31.1469573591066,10.));
#10534=CARTESIAN_POINT('Ctrl Pts',(37.6976185923575,31.1718010369838,10.));
#10535=CARTESIAN_POINT('Ctrl Pts',(37.7070512515414,31.1866409447872,10.));
#10536=CARTESIAN_POINT('Ctrl Pts',(37.7166325303773,31.2013762411221,10.));
#10537=CARTESIAN_POINT('Ctrl Pts',(37.7263603898849,31.2160016041003,10.));
#10538=CARTESIAN_POINT('Ctrl Pts',(37.7738890534039,31.2874586348368,10.));
#10539=CARTESIAN_POINT('Ctrl Pts',(37.8249264987974,31.3563136849385,10.));
#10540=CARTESIAN_POINT('Ctrl Pts',(37.8794383434655,31.4222140400578,10.));
#10541=CARTESIAN_POINT('Ctrl Pts',(37.9310244322697,31.4845773959873,10.));
#10542=CARTESIAN_POINT('Ctrl Pts',(37.9857224645776,31.5442949330007,10.));
#10543=CARTESIAN_POINT('Ctrl Pts',(38.0435270929093,31.6010318603323,10.));
#10544=CARTESIAN_POINT('Ctrl Pts',(38.0564930683829,31.6137583431323,10.));
#10545=CARTESIAN_POINT('Ctrl Pts',(38.069615433518,31.6263347020438,10.));
#10546=CARTESIAN_POINT('Ctrl Pts',(38.082890958175,31.6387596071244,10.));
#10547=CARTESIAN_POINT('Origin',(40.,-30.,12.2084234471775));
#10548=CARTESIAN_POINT('Ctrl Pts',(36.9237142109313,-29.9977821171135,9.70842344717746));
#10549=CARTESIAN_POINT('Ctrl Pts',(36.922516886621,-29.8529950058616,9.70090492237387));
#10550=CARTESIAN_POINT('Ctrl Pts',(36.9976394341993,-28.6901609317351,9.64045815782839));
#10551=CARTESIAN_POINT('Ctrl Pts',(38.4808974147036,-26.6996618505134,9.52708315354101));
#10552=CARTESIAN_POINT('Ctrl Pts',(41.9490299734334,-26.9342995801418,9.36829843431533));
#10553=CARTESIAN_POINT('Ctrl Pts',(43.6328192933167,-29.9750449290915,9.20951371508966));
#10554=CARTESIAN_POINT('Ctrl Pts',(41.9908418354334,-33.0388817878925,9.05072899586395));
#10555=CARTESIAN_POINT('Ctrl Pts',(38.5262719144904,-33.3205496312506,8.89194427663829));
#10556=CARTESIAN_POINT('Ctrl Pts',(37.0061629941113,-31.3385370033826,8.77784242707611));
#10557=CARTESIAN_POINT('Ctrl Pts',(36.9227280575122,-30.1612865754691,8.71666881725583));
#10558=CARTESIAN_POINT('Ctrl Pts',(36.9240972445879,-30.002414807271,8.70842344717746));
#10559=CARTESIAN_POINT('Ctrl Pts',(36.9295986129496,-30.0034658759783,9.79157655282254));
#10560=CARTESIAN_POINT('Ctrl Pts',(36.9349212216015,-29.2996636162424,9.75519455573124));
#10561=CARTESIAN_POINT('Ctrl Pts',(37.5227895751442,-27.5614666405174,9.66588431889804));
#10562=CARTESIAN_POINT('Ctrl Pts',(40.4091142364954,-26.3909769590634,9.52364584232295));
#10563=CARTESIAN_POINT('Ctrl Pts',(43.2541892892138,-28.3852504471766,9.36486112309727));
#10564=CARTESIAN_POINT('Ctrl Pts',(43.1213433300866,-31.8593327642316,9.20607640387157));
#10565=CARTESIAN_POINT('Ctrl Pts',(40.1303404283627,-33.6304598448459,9.04729168464591));
#10566=CARTESIAN_POINT('Ctrl Pts',(37.4241568402642,-32.2798861452479,8.90912506762956));
#10567=CARTESIAN_POINT('Ctrl Pts',(36.933714701829,-30.6241455749599,8.8238866903551));
#10568=CARTESIAN_POINT('Ctrl Pts',(36.9305018352452,-29.9982750548043,8.79157655282255));
#10569=CARTESIAN_POINT('Ctrl Pts',(41.9134659966651,-28.364012796625,10.));
#10570=CARTESIAN_POINT('Ctrl Pts',(42.4575265280738,-29.0003511034471,9.94707176025811));
#10571=CARTESIAN_POINT('Ctrl Pts',(42.8509955579937,-30.8479873408299,9.84121528077431));
#10572=CARTESIAN_POINT('Ctrl Pts',(40.8305801973719,-32.8592854911677,9.68243056154864));
#10573=CARTESIAN_POINT('Ctrl Pts',(38.0493536846231,-32.246350797925,9.52364584232294));
#10574=CARTESIAN_POINT('Ctrl Pts',(37.0541564286807,-29.5801373012942,9.36486112309728));
#10575=CARTESIAN_POINT('Ctrl Pts',(38.7557049752778,-27.2966971559029,9.20607640387158));
#10576=CARTESIAN_POINT('Ctrl Pts',(41.5964480097995,-27.4888886263241,9.04729168464589));
#10577=CARTESIAN_POINT('Ctrl Pts',(42.9756377325279,-29.9795593326787,8.88850696542022));
#10578=CARTESIAN_POINT('Ctrl Pts',(41.6306960535883,-32.489144265827,8.72972224619452));
#10579=CARTESIAN_POINT('Ctrl Pts',(38.7928711712151,-32.7198580434922,8.57093752696885));
#10580=CARTESIAN_POINT('Ctrl Pts',(37.0601567480849,-30.4606371277457,8.41215280774316));
#10581=CARTESIAN_POINT('Ctrl Pts',(38.0188182770251,-27.7796852899716,8.25336808851749));
#10582=CARTESIAN_POINT('Ctrl Pts',(40.7912199377621,-27.1314075284948,8.09458336929179));
#10583=CARTESIAN_POINT('Ctrl Pts',(42.8392723191738,-29.109272461031,7.93579865006612));
#10584=CARTESIAN_POINT('Ctrl Pts',(42.2880180434828,-31.9025869089777,7.77701393084043));
#10585=CARTESIAN_POINT('Ctrl Pts',(39.6421209206988,-32.9541128850707,7.61822921161475));
#10586=CARTESIAN_POINT('Ctrl Pts',(37.3238562454659,-31.3011981084002,7.45944449238906));
#10587=CARTESIAN_POINT('Ctrl Pts',(37.4555569385905,-28.4570575607117,7.30065977316338));
#10588=CARTESIAN_POINT('Ctrl Pts',(39.9166532379287,-27.0254555270554,7.14187505393769));
#10589=CARTESIAN_POINT('Ctrl Pts',(42.4540521133015,-28.316999721687,6.98309033471202));
#10590=CARTESIAN_POINT('Ctrl Pts',(42.7448068218058,-31.1493029192047,6.82430561548633));
#10591=CARTESIAN_POINT('Ctrl Pts',(40.522736224961,-32.9294382547638,6.66552089626065));
#10592=CARTESIAN_POINT('Ctrl Pts',(37.8221092503229,-32.0277212725262,6.50673617703495));
#10593=CARTESIAN_POINT('Ctrl Pts',(37.1153052795403,-29.2696589553355,6.34795145780928));
#10594=CARTESIAN_POINT('Ctrl Pts',(39.0493916727759,-27.1802118030299,6.18916673858359));
#10595=CARTESIAN_POINT('Ctrl Pts',(41.8537442861862,-27.6722341628753,6.03038201935791));
#10596=CARTESIAN_POINT('Ctrl Pts',(42.9610246280014,-30.2952876945972,5.87159730013222));
#10597=CARTESIAN_POINT('Ctrl Pts',(41.3575358365671,-32.6480102194343,5.71281258090655));
#10598=CARTESIAN_POINT('Ctrl Pts',(38.5112454121581,-32.5765231315497,5.55402786168086));
#10599=CARTESIAN_POINT('Ctrl Pts',(37.0278852198967,-30.1462716786976,5.39524314245518));
#10600=CARTESIAN_POINT('Ctrl Pts',(38.2654470119066,-27.5821109203365,5.23645842322949));
#10601=CARTESIAN_POINT('Ctrl Pts',(41.090963411111,-27.2314876728225,5.07767370400381));
#10602=CARTESIAN_POINT('Ctrl Pts',(42.917720829271,-29.415391727283,4.91888898477813));
#10603=CARTESIAN_POINT('Ctrl Pts',(42.0733530266078,-32.1344949981544,4.76010426555244));
#10604=CARTESIAN_POINT('Ctrl Pts',(39.3308647781861,-32.8995033583434,4.60131954632676));
#10605=CARTESIAN_POINT('Ctrl Pts',(37.2009587717734,-31.0100642913931,4.44253482710107));
#10606=CARTESIAN_POINT('Ctrl Pts',(37.6335287719039,-28.1959280511325,4.28375010787539));
#10607=CARTESIAN_POINT('Ctrl Pts',(40.2325640892091,-27.033389878221,4.12496538864971));
#10608=CARTESIAN_POINT('Ctrl Pts',(42.6186908245506,-28.5867342658908,3.96618066942403));
#10609=CARTESIAN_POINT('Ctrl Pts',(42.6074493687812,-31.4339000869844,3.80739595019834));
#10610=CARTESIAN_POINT('Ctrl Pts',(40.2091310885856,-32.9683540656127,3.64861123097266));
#10611=CARTESIAN_POINT('Ctrl Pts',(37.6193567519611,-31.7853289313531,3.48982651174698));
#10612=CARTESIAN_POINT('Ctrl Pts',(37.2090219816371,-28.9678646538439,3.33104179252129));
#10613=CARTESIAN_POINT('Ctrl Pts',(39.3537814844175,-27.0953032332612,3.17225707329561));
#10614=CARTESIAN_POINT('Ctrl Pts',(42.0901433592587,-27.8819437242824,3.01347235406992));
#10615=CARTESIAN_POINT('Ctrl Pts',(42.9130135240572,-30.6076297374087,2.85468763484424));
#10616=CARTESIAN_POINT('Ctrl Pts',(41.0690679124311,-32.7770407829578,2.69590291561856));
#10617=CARTESIAN_POINT('Ctrl Pts',(38.2464083185899,-32.4041168272699,2.53711819639287));
#10618=CARTESIAN_POINT('Ctrl Pts',(37.0291328782873,-29.8302637079522,2.37833347716719));
#10619=CARTESIAN_POINT('Ctrl Pts',(38.5316373372112,-27.4118012049374,2.21954875794151));
#10620=CARTESIAN_POINT('Ctrl Pts',(41.3784033068818,-27.3627922537806,2.06076403871582));
#10621=CARTESIAN_POINT('Ctrl Pts',(42.9632643203048,-29.7281028107449,1.90197931949014));
#10622=CARTESIAN_POINT('Ctrl Pts',(41.8353047983154,-32.3423319893612,1.74319460026446));
#10623=CARTESIAN_POINT('Ctrl Pts',(39.0271560503567,-32.812192455564,1.58440988103877));
#10624=CARTESIAN_POINT('Ctrl Pts',(37.1096258746627,-30.7075421164847,1.42562516181309));
#10625=CARTESIAN_POINT('Ctrl Pts',(37.838193439687,-27.9551388054256,1.2668404425874));
#10626=CARTESIAN_POINT('Ctrl Pts',(40.5458432691404,-27.0747918173971,1.10805572336172));
#10627=CARTESIAN_POINT('Ctrl Pts',(42.7538144212495,-28.872385292484,0.949271004136037));
#10628=CARTESIAN_POINT('Ctrl Pts',(42.4406504077013,-31.7023699138296,0.790486284910354));
#10629=CARTESIAN_POINT('Ctrl Pts',(39.8932382042214,-32.9737061889096,0.631701565684669));
#10630=CARTESIAN_POINT('Ctrl Pts',(37.4433111114008,-31.5229767898314,0.472916846458986));
#10631=CARTESIAN_POINT('Ctrl Pts',(37.3344969165913,-28.6773615971149,0.314132127233303));
#10632=CARTESIAN_POINT('Ctrl Pts',(39.6648949029946,-27.0438508953382,0.155347408007618));
#10633=CARTESIAN_POINT('Ctrl Pts',(42.3041007393156,-28.1141323568833,-0.00343731121806418));
#10634=CARTESIAN_POINT('Ctrl Pts',(42.8298462181864,-30.9160942000275,-0.162222030443749));
#10635=CARTESIAN_POINT('Ctrl Pts',(41.4590097705807,-32.2158576312381,-0.268078509927538));
#10636=CARTESIAN_POINT('Ctrl Pts',(40.6501999979751,-32.4320868020351,-0.321006749669432));
#10637=CARTESIAN_POINT('Ctrl Pts',(42.0543315503421,-28.2435746787731,10.1070022498898));
#10638=CARTESIAN_POINT('Ctrl Pts',(42.6384447339141,-28.9267589437008,10.0540740101479));
#10639=CARTESIAN_POINT('Ctrl Pts',(43.0608801697441,-30.9104144790625,9.94821753066413));
#10640=CARTESIAN_POINT('Ctrl Pts',(40.8917258563906,-33.0697803912789,9.78943281143844));
#10641=CARTESIAN_POINT('Ctrl Pts',(37.9057509899724,-32.4117226673253,9.63064809221276));
#10642=CARTESIAN_POINT('Ctrl Pts',(36.8372892951947,-29.5492278460832,9.47186337298707));
#10643=CARTESIAN_POINT('Ctrl Pts',(38.6641024550864,-27.0976853874398,9.3130786537614));
#10644=CARTESIAN_POINT('Ctrl Pts',(41.7139753310108,-27.30402561093,9.1542939345357));
#10645=CARTESIAN_POINT('Ctrl Pts',(43.1946982527908,-29.9780545314829,8.99550921531004));
#10646=CARTESIAN_POINT('Ctrl Pts',(41.7507446475367,-32.6723901065155,8.83672449608433));
#10647=CARTESIAN_POINT('Ctrl Pts',(38.7040047523069,-32.920088572745,8.67793977685867));
#10648=CARTESIAN_POINT('Ctrl Pts',(36.8437313461564,-30.4945483151706,8.51915505763297));
#10649=CARTESIAN_POINT('Ctrl Pts',(37.8729676265154,-27.6162301454795,8.3603703384073));
#10650=CARTESIAN_POINT('Ctrl Pts',(40.8494679729022,-26.9202274670375,8.2015856191816));
#10651=CARTESIAN_POINT('Ctrl Pts',(43.0482938894434,-29.0436988745806,8.04280089995593));
#10652=CARTESIAN_POINT('Ctrl Pts',(42.45645737247,-32.0426515658982,7.88401618073024));
#10653=CARTESIAN_POINT('Ctrl Pts',(39.6157745760326,-33.1715887889567,7.72523146150456));
#10654=CARTESIAN_POINT('Ctrl Pts',(37.126843875056,-31.3969897202202,7.56644674227887));
#10655=CARTESIAN_POINT('Ctrl Pts',(37.2682401107661,-28.3434692129799,7.40766202305318));
#10656=CARTESIAN_POINT('Ctrl Pts',(39.9105174153916,-26.8064754903845,7.24887730382751));
#10657=CARTESIAN_POINT('Ctrl Pts',(42.6347145396498,-28.193100594942,7.09009258460182));
#10658=CARTESIAN_POINT('Ctrl Pts',(42.9468740304021,-31.2339123098803,6.93130786537613));
#10659=CARTESIAN_POINT('Ctrl Pts',(40.561219024177,-33.1450976615362,6.77252314615046));
#10660=CARTESIAN_POINT('Ctrl Pts',(37.6617772732529,-32.1769980719337,6.61373842692477));
#10661=CARTESIAN_POINT('Ctrl Pts',(36.9029398026022,-29.2158927029908,6.45495370769909));
#10662=CARTESIAN_POINT('Ctrl Pts',(38.9794097820196,-26.9726246150106,6.2961689884734));
#10663=CARTESIAN_POINT('Ctrl Pts',(41.9902132465463,-27.5008686805263,6.13738426924773));
#10664=CARTESIAN_POINT('Ctrl Pts',(43.1790093606288,-30.3170261862484,5.97859955002204));
#10665=CARTESIAN_POINT('Ctrl Pts',(41.4574749196696,-32.8429514550524,5.81981483079635));
#10666=CARTESIAN_POINT('Ctrl Pts',(38.4016462660687,-32.7662016302113,5.66103011157067));
#10667=CARTESIAN_POINT('Ctrl Pts',(36.809084052371,-30.1570399082051,5.50224539234499));
#10668=CARTESIAN_POINT('Ctrl Pts',(38.1377526773975,-27.4041107444619,5.3434606731193));
#10669=CARTESIAN_POINT('Ctrl Pts',(41.1712779634549,-27.0276753121591,5.18467595389362));
#10670=CARTESIAN_POINT('Ctrl Pts',(43.1325176225281,-29.3723540312048,5.02589123466794));
#10671=CARTESIAN_POINT('Ctrl Pts',(42.2259891448195,-32.2916322664727,4.86710651544225));
#10672=CARTESIAN_POINT('Ctrl Pts',(39.2816043765537,-33.1129590176931,4.70832179621657));
#10673=CARTESIAN_POINT('Ctrl Pts',(36.9948989342501,-31.0844232117526,4.54953707699089));
#10674=CARTESIAN_POINT('Ctrl Pts',(37.4593138758004,-28.0631158692628,4.3907523577652));
#10675=CARTESIAN_POINT('Ctrl Pts',(40.2496849940221,-26.814993952672,4.23196763853952));
#10676=CARTESIAN_POINT('Ctrl Pts',(42.8114736247426,-28.4826924587852,4.07318291931384));
#10677=CARTESIAN_POINT('Ctrl Pts',(42.7994045954005,-31.5394609540302,3.91439820008815));
#10678=CARTESIAN_POINT('Ctrl Pts',(40.224526902588,-33.1868783768316,3.75561348086247));
#10679=CARTESIAN_POINT('Ctrl Pts',(37.4440985399902,-31.9167612896229,3.59682876163679));
#10680=CARTESIAN_POINT('Ctrl Pts',(37.0035557415564,-28.8918809064142,3.4380440424111));
#10681=CARTESIAN_POINT('Ctrl Pts',(39.3062081650313,-26.8814652455344,3.27925932318542));
#10682=CARTESIAN_POINT('Ctrl Pts',(42.2440155483017,-27.7260166419522,3.12047460395973));
#10683=CARTESIAN_POINT('Ctrl Pts',(43.1274637748849,-30.6523622278423,2.96168988473405));
#10684=CARTESIAN_POINT('Ctrl Pts',(41.1477705617938,-32.9814809915411,2.80290516550837));
#10685=CARTESIAN_POINT('Ctrl Pts',(38.1173123934176,-32.5811031173675,2.64412044628268));
#10686=CARTESIAN_POINT('Ctrl Pts',(36.8104235608861,-29.8177680603682,2.485335727057));
#10687=CARTESIAN_POINT('Ctrl Pts',(38.4235394040089,-27.2212631671942,2.32655100783132));
#10688=CARTESIAN_POINT('Ctrl Pts',(41.4798786115659,-27.1686462747144,2.16776628860563));
#10689=CARTESIAN_POINT('Ctrl Pts',(43.1814139346165,-29.7080862814863,2.00898156937995));
#10690=CARTESIAN_POINT('Ctrl Pts',(41.9704162803231,-32.5147698028117,1.85019685015426));
#10691=CARTESIAN_POINT('Ctrl Pts',(38.9555372173872,-33.0192204602371,1.69141213092858));
#10692=CARTESIAN_POINT('Ctrl Pts',(36.8968422912549,-30.7596299571687,1.5326274117029));
#10693=CARTESIAN_POINT('Ctrl Pts',(37.6790455485868,-27.804600199112,1.37384269247721));
#10694=CARTESIAN_POINT('Ctrl Pts',(40.586027162903,-26.8594438201078,1.21505797325153));
#10695=CARTESIAN_POINT('Ctrl Pts',(42.9565447513674,-28.7893725447344,1.05627325402585));
#10696=CARTESIAN_POINT('Ctrl Pts',(42.6203262271891,-31.8276949945432,0.897488534800166));
#10697=CARTESIAN_POINT('Ctrl Pts',(39.8853786135623,-33.1926245127803,0.738703815574479));
#10698=CARTESIAN_POINT('Ctrl Pts',(37.2550927701812,-31.6350953062361,0.579919096348798));
#10699=CARTESIAN_POINT('Ctrl Pts',(37.1382678911857,-28.5799915935394,0.421134377123113));
#10700=CARTESIAN_POINT('Ctrl Pts',(39.640225133523,-26.8262250890235,0.262349657897429));
#10701=CARTESIAN_POINT('Ctrl Pts',(42.4737240443217,-27.9752985389988,0.103564938671746));
#10702=CARTESIAN_POINT('Ctrl Pts',(43.0381738576848,-30.9835352295164,-0.0552197805539384));
#10703=CARTESIAN_POINT('Ctrl Pts',(41.5664191624963,-32.3789846544712,-0.161076260037727));
#10704=CARTESIAN_POINT('Ctrl Pts',(40.698066426161,-32.6111321859386,-0.214004499779622));
#10705=CARTESIAN_POINT('Ctrl Pts',(42.1951971040191,-28.1231365609212,10.2140044997796));
#10706=CARTESIAN_POINT('Ctrl Pts',(42.8193629397544,-28.8531667839546,10.1610762600377));
#10707=CARTESIAN_POINT('Ctrl Pts',(43.2707647814944,-30.9728416172951,10.0552197805539));
#10708=CARTESIAN_POINT('Ctrl Pts',(40.9528715154093,-33.28027529139,9.89643506132827));
#10709=CARTESIAN_POINT('Ctrl Pts',(37.7621482953217,-32.5770945367257,9.73765034210256));
#10710=CARTESIAN_POINT('Ctrl Pts',(36.6204221617086,-29.5183183908723,9.57886562287689));
#10711=CARTESIAN_POINT('Ctrl Pts',(38.572499934895,-26.8986736189766,9.4200809036512));
#10712=CARTESIAN_POINT('Ctrl Pts',(41.8315026522221,-27.1191625955359,9.26129618442551));
#10713=CARTESIAN_POINT('Ctrl Pts',(43.4137587730538,-29.9765497302872,9.10251146519984));
#10714=CARTESIAN_POINT('Ctrl Pts',(41.8707932414851,-32.855635947204,8.94372674597415));
#10715=CARTESIAN_POINT('Ctrl Pts',(38.6151383333986,-33.1203191019978,8.78494202674847));
#10716=CARTESIAN_POINT('Ctrl Pts',(36.6273059442279,-30.5284595025955,8.62615730752278));
#10717=CARTESIAN_POINT('Ctrl Pts',(37.7271169760057,-27.4527750009875,8.46737258829711));
#10718=CARTESIAN_POINT('Ctrl Pts',(40.9077160080424,-26.7090474055801,8.30858786907142));
#10719=CARTESIAN_POINT('Ctrl Pts',(43.2573154597129,-28.9781252881302,8.14980314984573));
#10720=CARTESIAN_POINT('Ctrl Pts',(42.6248967014573,-32.1827162228186,7.99101843062006));
#10721=CARTESIAN_POINT('Ctrl Pts',(39.5894282313664,-33.3890646928428,7.83223371139436));
#10722=CARTESIAN_POINT('Ctrl Pts',(36.9298315046461,-31.4927813320402,7.67344899216869));
#10723=CARTESIAN_POINT('Ctrl Pts',(37.0809232829417,-28.2298808652481,7.514664272943));
#10724=CARTESIAN_POINT('Ctrl Pts',(39.9043815928545,-26.5874954537136,7.35587955371732));
#10725=CARTESIAN_POINT('Ctrl Pts',(42.8153769659981,-28.069201468197,7.19709483449164));
#10726=CARTESIAN_POINT('Ctrl Pts',(43.1489412389985,-31.3185217005559,7.03831011526595));
#10727=CARTESIAN_POINT('Ctrl Pts',(40.5997018233928,-33.3607570683086,6.87952539604027));
#10728=CARTESIAN_POINT('Ctrl Pts',(37.501445296183,-32.326274871341,6.72074067681458));
#10729=CARTESIAN_POINT('Ctrl Pts',(36.690574325664,-29.1621264506462,6.5619559575889));
#10730=CARTESIAN_POINT('Ctrl Pts',(38.9094278912633,-26.7650374269914,6.40317123836322));
#10731=CARTESIAN_POINT('Ctrl Pts',(42.1266822069064,-27.3295031981772,6.24438651913754));
#10732=CARTESIAN_POINT('Ctrl Pts',(43.3969940932563,-30.3387646778996,6.08560179991185));
#10733=CARTESIAN_POINT('Ctrl Pts',(41.557414002772,-33.0378926906704,5.92681708068617));
#10734=CARTESIAN_POINT('Ctrl Pts',(38.2920471199794,-32.9558801288729,5.76803236146048));
#10735=CARTESIAN_POINT('Ctrl Pts',(36.5902828848454,-30.1678081377126,5.6092476422348));
#10736=CARTESIAN_POINT('Ctrl Pts',(38.0100583428884,-27.2261105685873,5.45046292300911));
#10737=CARTESIAN_POINT('Ctrl Pts',(41.2515925157989,-26.8238629514956,5.29167820378343));
#10738=CARTESIAN_POINT('Ctrl Pts',(43.3473144157852,-29.3293163351266,5.13289348455775));
#10739=CARTESIAN_POINT('Ctrl Pts',(42.3786252630313,-32.4487695347909,4.97410876533207));
#10740=CARTESIAN_POINT('Ctrl Pts',(39.2323439749213,-33.3264146770428,4.81532404610638));
#10741=CARTESIAN_POINT('Ctrl Pts',(36.788839096727,-31.158782132112,4.6565393268807));
#10742=CARTESIAN_POINT('Ctrl Pts',(37.285098979697,-27.9303036873932,4.49775460765501));
#10743=CARTESIAN_POINT('Ctrl Pts',(40.266805898835,-26.596598027123,4.33896988842933));
#10744=CARTESIAN_POINT('Ctrl Pts',(43.0042564249346,-28.3786506516797,4.18018516920364));
#10745=CARTESIAN_POINT('Ctrl Pts',(42.9913598220198,-31.645021821076,4.02140044997796));
#10746=CARTESIAN_POINT('Ctrl Pts',(40.2399227165905,-33.4054026880505,3.86261573075228));
#10747=CARTESIAN_POINT('Ctrl Pts',(37.2688403280194,-32.0481936478926,3.7038310115266));
#10748=CARTESIAN_POINT('Ctrl Pts',(36.7980895014757,-28.8158971589845,3.54504629230091));
#10749=CARTESIAN_POINT('Ctrl Pts',(39.2586348456451,-26.6676272578076,3.38626157307523));
#10750=CARTESIAN_POINT('Ctrl Pts',(42.3978877373448,-27.5700895596219,3.22747685384954));
#10751=CARTESIAN_POINT('Ctrl Pts',(43.3419140257126,-30.6970947182758,3.06869213462386));
#10752=CARTESIAN_POINT('Ctrl Pts',(41.2264732111564,-33.1859212001242,2.90990741539818));
#10753=CARTESIAN_POINT('Ctrl Pts',(37.9882164682452,-32.7580894074651,2.75112269617249));
#10754=CARTESIAN_POINT('Ctrl Pts',(36.591714243485,-29.8052724127842,2.59233797694681));
#10755=CARTESIAN_POINT('Ctrl Pts',(38.3154414708065,-27.0307251294511,2.43355325772113));
#10756=CARTESIAN_POINT('Ctrl Pts',(41.5813539162499,-26.9745002956481,2.27476853849544));
#10757=CARTESIAN_POINT('Ctrl Pts',(43.3995635489283,-29.6880697522276,2.11598381926976));
#10758=CARTESIAN_POINT('Ctrl Pts',(42.1055277623309,-32.6872076162622,1.95719910004408));
#10759=CARTESIAN_POINT('Ctrl Pts',(38.8839183844178,-33.2262484649101,1.79841438081839));
#10760=CARTESIAN_POINT('Ctrl Pts',(36.6840587078471,-30.8117177978527,1.63962966159271));
#10761=CARTESIAN_POINT('Ctrl Pts',(37.5198976574866,-27.6540615927984,1.48084494236703));
#10762=CARTESIAN_POINT('Ctrl Pts',(40.6262110566655,-26.6440958228186,1.32206022314134));
#10763=CARTESIAN_POINT('Ctrl Pts',(43.1592750814852,-28.7063597969847,1.16327550391566));
#10764=CARTESIAN_POINT('Ctrl Pts',(42.8000020466769,-31.9530200752568,1.00449078468998));
#10765=CARTESIAN_POINT('Ctrl Pts',(39.8775190229031,-33.411542836651,0.84570606546429));
#10766=CARTESIAN_POINT('Ctrl Pts',(37.0668744289616,-31.7472138226408,0.686921346238608));
#10767=CARTESIAN_POINT('Ctrl Pts',(36.9420388657802,-28.4826215899638,0.528136627012925));
#10768=CARTESIAN_POINT('Ctrl Pts',(39.6155553640513,-26.6085992827088,0.369351907787239));
#10769=CARTESIAN_POINT('Ctrl Pts',(42.6433473493279,-27.8364647211143,0.210567188561557));
#10770=CARTESIAN_POINT('Ctrl Pts',(43.2465014971832,-31.0509762590054,0.0517824693358723));
#10771=CARTESIAN_POINT('Ctrl Pts',(41.673828554412,-32.5421116777044,-0.0540740101479163));
#10772=CARTESIAN_POINT('Ctrl Pts',(40.7459328543469,-32.7901775698422,-0.107002249889811));
#10773=CARTESIAN_POINT('Ctrl Pts',(42.3360626576962,-28.0026984430693,10.3210067496694));
#10774=CARTESIAN_POINT('Ctrl Pts',(43.0002811455947,-28.7795746242084,10.2680785099275));
#10775=CARTESIAN_POINT('Ctrl Pts',(43.4806493932448,-31.0352687555276,10.1622220304437));
#10776=CARTESIAN_POINT('Ctrl Pts',(41.014017174428,-33.4907701915011,10.0034373112181));
#10777=CARTESIAN_POINT('Ctrl Pts',(37.6185456006709,-32.7424664061261,9.84465259199238));
#10778=CARTESIAN_POINT('Ctrl Pts',(36.4035550282225,-29.4874089356614,9.68586787276671));
#10779=CARTESIAN_POINT('Ctrl Pts',(38.4808974147036,-26.6996618505134,9.52708315354101));
#10780=CARTESIAN_POINT('Ctrl Pts',(41.9490299734334,-26.9342995801418,9.36829843431533));
#10781=CARTESIAN_POINT('Ctrl Pts',(43.6328192933167,-29.9750449290915,9.20951371508966));
#10782=CARTESIAN_POINT('Ctrl Pts',(41.9908418354334,-33.0388817878925,9.05072899586395));
#10783=CARTESIAN_POINT('Ctrl Pts',(38.5262719144904,-33.3205496312506,8.89194427663829));
#10784=CARTESIAN_POINT('Ctrl Pts',(36.4108805422994,-30.5623706900205,8.73315955741259));
#10785=CARTESIAN_POINT('Ctrl Pts',(37.5812663254961,-27.2893198564955,8.57437483818692));
#10786=CARTESIAN_POINT('Ctrl Pts',(40.9659640431824,-26.4978673441227,8.41559011896122));
#10787=CARTESIAN_POINT('Ctrl Pts',(43.4663370299824,-28.9125517016798,8.25680539973555));
#10788=CARTESIAN_POINT('Ctrl Pts',(42.7933360304446,-32.322780879739,8.09802068050986));
#10789=CARTESIAN_POINT('Ctrl Pts',(39.5630818867002,-33.6065405967288,7.93923596128418));
#10790=CARTESIAN_POINT('Ctrl Pts',(36.7328191342362,-31.5885729438602,7.7804512420585));
#10791=CARTESIAN_POINT('Ctrl Pts',(36.8936064551174,-28.1162925175164,7.62166652283281));
#10792=CARTESIAN_POINT('Ctrl Pts',(39.8982457703173,-26.3685154170426,7.46288180360713));
#10793=CARTESIAN_POINT('Ctrl Pts',(42.9960393923464,-27.9453023414519,7.30409708438144));
#10794=CARTESIAN_POINT('Ctrl Pts',(43.3510084475949,-31.4031310912316,7.14531236515576));
#10795=CARTESIAN_POINT('Ctrl Pts',(40.6381846226088,-33.576416475081,6.98652764593008));
#10796=CARTESIAN_POINT('Ctrl Pts',(37.3411133191131,-32.4755516707485,6.82774292670439));
#10797=CARTESIAN_POINT('Ctrl Pts',(36.4782088487258,-29.1083601983015,6.66895820747871));
#10798=CARTESIAN_POINT('Ctrl Pts',(38.8394460005071,-26.5574502389721,6.51017348825302));
#10799=CARTESIAN_POINT('Ctrl Pts',(42.2631511672664,-27.1581377158282,6.35138876902735));
#10800=CARTESIAN_POINT('Ctrl Pts',(43.6149788258837,-30.3605031695509,6.19260404980166));
#10801=CARTESIAN_POINT('Ctrl Pts',(41.6573530858745,-33.2328339262885,6.03381933057598));
#10802=CARTESIAN_POINT('Ctrl Pts',(38.1824479738899,-33.1455586275345,5.87503461135029));
#10803=CARTESIAN_POINT('Ctrl Pts',(36.3714817173198,-30.1785763672202,5.7162498921246));
#10804=CARTESIAN_POINT('Ctrl Pts',(37.8823640083793,-27.0481103927127,5.55746517289893));
#10805=CARTESIAN_POINT('Ctrl Pts',(41.3319070681429,-26.6200505908322,5.39868045367324));
#10806=CARTESIAN_POINT('Ctrl Pts',(43.5621112090423,-29.2862786390484,5.23989573444757));
#10807=CARTESIAN_POINT('Ctrl Pts',(42.531261381243,-32.6059068031093,5.08111101522187));
#10808=CARTESIAN_POINT('Ctrl Pts',(39.1830835732889,-33.5398703363926,4.92232629599619));
#10809=CARTESIAN_POINT('Ctrl Pts',(36.5827792592038,-31.2331410524714,4.76354157677051));
#10810=CARTESIAN_POINT('Ctrl Pts',(37.1108840835935,-27.7974915055236,4.60475685754483));
#10811=CARTESIAN_POINT('Ctrl Pts',(40.2839268036481,-26.3782021015739,4.44597213831914));
#10812=CARTESIAN_POINT('Ctrl Pts',(43.1970392251266,-28.2746088445741,4.28718741909346));
#10813=CARTESIAN_POINT('Ctrl Pts',(43.1833150486392,-31.7505826881217,4.12840269986777));
#10814=CARTESIAN_POINT('Ctrl Pts',(40.2553185305929,-33.6239269992694,3.9696179806421));
#10815=CARTESIAN_POINT('Ctrl Pts',(37.0935821160486,-32.1796260061624,3.8108332614164));
#10816=CARTESIAN_POINT('Ctrl Pts',(36.5926232613949,-28.7399134115548,3.65204854219073));
#10817=CARTESIAN_POINT('Ctrl Pts',(39.211061526259,-26.4537892700808,3.49326382296504));
#10818=CARTESIAN_POINT('Ctrl Pts',(42.5517599263879,-27.4141624772917,3.33447910373936));
#10819=CARTESIAN_POINT('Ctrl Pts',(43.5563642765403,-30.7418272087093,3.17569438451367));
#10820=CARTESIAN_POINT('Ctrl Pts',(41.3051758605191,-33.3903614087074,3.01690966528799));
#10821=CARTESIAN_POINT('Ctrl Pts',(37.8591205430729,-32.9350756975626,2.8581249460623));
#10822=CARTESIAN_POINT('Ctrl Pts',(36.3730049260838,-29.7927767652001,2.69934022683663));
#10823=CARTESIAN_POINT('Ctrl Pts',(38.2073435376042,-26.840187091708,2.54055550761094));
#10824=CARTESIAN_POINT('Ctrl Pts',(41.682829220934,-26.7803543165819,2.38177078838526));
#10825=CARTESIAN_POINT('Ctrl Pts',(43.61771316324,-29.668053222969,2.22298606915957));
#10826=CARTESIAN_POINT('Ctrl Pts',(42.2406392443386,-32.8596454297127,2.06420134993389));
#10827=CARTESIAN_POINT('Ctrl Pts',(38.8122995514484,-33.4332764695832,1.9054166307082));
#10828=CARTESIAN_POINT('Ctrl Pts',(36.4712751244393,-30.8638056385366,1.74663191148252));
#10829=CARTESIAN_POINT('Ctrl Pts',(37.3607497663865,-27.5035229864848,1.58784719225684));
#10830=CARTESIAN_POINT('Ctrl Pts',(40.6663949504281,-26.4287478255293,1.42906247303115));
#10831=CARTESIAN_POINT('Ctrl Pts',(43.362005411603,-28.6233470492352,1.27027775380547));
#10832=CARTESIAN_POINT('Ctrl Pts',(42.9796778661648,-32.0783451559703,1.11149303457979));
#10833=CARTESIAN_POINT('Ctrl Pts',(39.869659432244,-33.6304611605218,0.952708315354101));
#10834=CARTESIAN_POINT('Ctrl Pts',(36.878656087742,-31.8593323390454,0.793923596128419));
#10835=CARTESIAN_POINT('Ctrl Pts',(36.7458098403747,-28.3852515863884,0.635138876902735));
#10836=CARTESIAN_POINT('Ctrl Pts',(39.5908855945796,-26.390973476394,0.47635415767705));
#10837=CARTESIAN_POINT('Ctrl Pts',(42.8129706543341,-27.6976309032298,0.317569438451368));
#10838=CARTESIAN_POINT('Ctrl Pts',(43.4548291366816,-31.1184172884943,0.158784719225683));
#10839=CARTESIAN_POINT('Ctrl Pts',(41.7812379463276,-32.7052387009375,0.0529282397418946));
#10840=CARTESIAN_POINT('Ctrl Pts',(40.7937992825329,-32.9692229537457,0.));
#10841=CARTESIAN_POINT('Ctrl Pts',(40.7937992825329,-32.9692229537457,0.));
#10842=CARTESIAN_POINT('Ctrl Pts',(40.8868533414383,-32.9351833633283,-2.56313906977734E-16));
#10843=CARTESIAN_POINT('Ctrl Pts',(40.9778401769864,-32.8963743202609,7.1182815471101E-16));
#10844=CARTESIAN_POINT('Ctrl Pts',(41.0665520083656,-32.8531245549121,6.10622663543836E-16));
#10845=CARTESIAN_POINT('Ctrl Pts',(41.1572336482529,-32.8089144469075,5.07169947463599E-16));
#10846=CARTESIAN_POINT('Ctrl Pts',(41.2455387982709,-32.7600636012823,2.44567181551013E-15));
#10847=CARTESIAN_POINT('Ctrl Pts',(41.3312165904369,-32.7068775829945,2.72004641033163E-15));
#10848=CARTESIAN_POINT('Ctrl Pts',(41.4141659908734,-32.655385262557,2.98568360242218E-15));
#10849=CARTESIAN_POINT('Ctrl Pts',(41.4946530297383,-32.5998286158413,1.76977927080473E-15));
#10850=CARTESIAN_POINT('Ctrl Pts',(41.572416340159,-32.5404542465392,1.99840144432528E-15));
#10851=CARTESIAN_POINT('Ctrl Pts',(41.6404592367772,-32.4885016733999,2.19844584615577E-15));
#10852=CARTESIAN_POINT('Ctrl Pts',(41.7064164820401,-32.4336254394482,-4.49373757059322E-16));
#10853=CARTESIAN_POINT('Ctrl Pts',(41.7700877162758,-32.3759777741253,-5.55111512312578E-16));
#10854=CARTESIAN_POINT('Ctrl Pts',(41.7834303267024,-32.3638974312572,-5.7726936259868E-16));
#10855=CARTESIAN_POINT('Ctrl Pts',(41.796674321218,-32.3516934837044,-1.58746591514753E-15));
#10856=CARTESIAN_POINT('Ctrl Pts',(41.8098006766232,-32.3393836364141,-1.60982338570648E-15));
#10857=CARTESIAN_POINT('Ctrl Pts',(41.8822282662216,-32.2714613122024,-1.73318570922317E-15));
#10858=CARTESIAN_POINT('Ctrl Pts',(41.9511901377659,-32.2002177731016,-2.93438087003687E-15));
#10859=CARTESIAN_POINT('Ctrl Pts',(42.0164469480358,-32.1259441928838,-2.94209101525666E-15));
#10860=CARTESIAN_POINT('Ctrl Pts',(42.0813424310536,-32.0520818658139,-2.9497584693677E-15));
#10861=CARTESIAN_POINT('Ctrl Pts',(42.1425742542194,-31.9752221613491,-1.88528885175235E-15));
#10862=CARTESIAN_POINT('Ctrl Pts',(42.1998634141426,-31.8956246979978,-2.3037127760972E-15));
#10863=CARTESIAN_POINT('Ctrl Pts',(42.2557185048177,-31.8180197280708,-2.71166266166342E-15));
#10864=CARTESIAN_POINT('Ctrl Pts',(42.3078261181292,-31.7378116076102,2.65808508142602E-16));
#10865=CARTESIAN_POINT('Ctrl Pts',(42.3558808204457,-31.6552268221773,2.77555756156289E-16));
#10866=CARTESIAN_POINT('Ctrl Pts',(42.3766084052719,-31.6196052687622,2.8262273332898E-16));
#10867=CARTESIAN_POINT('Ctrl Pts',(42.396581328328,-31.5835414239387,-1.13197147658776E-15));
#10868=CARTESIAN_POINT('Ctrl Pts',(42.4157720959317,-31.5470531303214,-9.15933995315754E-16));
#10869=CARTESIAN_POINT('Ctrl Pts',(42.4294374934211,-31.5210704783355,-7.62097623829557E-16));
#10870=CARTESIAN_POINT('Ctrl Pts',(42.4427062526566,-31.494872601805,-2.6961316652602E-15));
#10871=CARTESIAN_POINT('Ctrl Pts',(42.4555678499899,-31.4684659394331,-2.85882428840978E-15));
#10872=CARTESIAN_POINT('Ctrl Pts',(42.461183367079,-31.4569364956189,-2.92985770532468E-15));
#10873=CARTESIAN_POINT('Ctrl Pts',(42.466720339292,-31.4453690485835,-5.42172902776515E-15));
#10874=CARTESIAN_POINT('Ctrl Pts',(42.4721741965263,-31.4337724107416,-5.32907051820075E-15));
#10875=CARTESIAN_POINT('Ctrl Pts',(42.5124020269377,-31.3482352284496,-4.64561830286583E-15));
#10876=CARTESIAN_POINT('Ctrl Pts',(42.5481738190905,-31.2609849169841,-3.53734486715838E-18));
#10877=CARTESIAN_POINT('Ctrl Pts',(42.5792385941522,-31.1722587986469,1.66533453693773E-16));
#10878=CARTESIAN_POINT('Ctrl Pts',(42.609616658182,-31.085494040215,3.32844704878679E-16));
#10879=CARTESIAN_POINT('Ctrl Pts',(42.6354937269254,-30.9973173268531,1.38062588022343E-15));
#10880=CARTESIAN_POINT('Ctrl Pts',(42.6565859822745,-30.907941771704,2.22044604925031E-15));
#10881=CARTESIAN_POINT('Ctrl Pts',(42.6603146190692,-30.8921421818565,2.36890738405432E-15));
#10882=CARTESIAN_POINT('Ctrl Pts',(42.6638935978244,-30.8763051196421,-1.87440975142009E-15));
#10883=CARTESIAN_POINT('Ctrl Pts',(42.6673211784214,-30.8604317567702,-1.99840144432528E-15));
#10884=CARTESIAN_POINT('Ctrl Pts',(42.6874320816035,-30.7672967728217,-2.78141844429488E-15));
#10885=CARTESIAN_POINT('Ctrl Pts',(42.7023350183962,-30.6729110567368,3.99432902596115E-17));
#10886=CARTESIAN_POINT('Ctrl Pts',(42.7121084797748,-30.5776835032973,-6.66133814775094E-16));
#10887=CARTESIAN_POINT('Ctrl Pts',(42.7153863724595,-30.5457454121019,-9.02942954116546E-16));
#10888=CARTESIAN_POINT('Ctrl Pts',(42.7180868619563,-30.513712748472,9.49954623796192E-16));
#10889=CARTESIAN_POINT('Ctrl Pts',(42.7202116846012,-30.4816014077219,1.11022302462516E-15));
#10890=CARTESIAN_POINT('Ctrl Pts',(42.7214003069685,-30.4636383753964,1.19987691006264E-15));
#10891=CARTESIAN_POINT('Ctrl Pts',(42.7224087772442,-30.4456507281831,-1.70559861591596E-15));
#10892=CARTESIAN_POINT('Ctrl Pts',(42.7232373200213,-30.4276412935577,-1.77635683940025E-15));
#10893=CARTESIAN_POINT('Ctrl Pts',(42.723811587505,-30.415158856935,-1.82539974710676E-15));
#10894=CARTESIAN_POINT('Ctrl Pts',(42.7242993034867,-30.4026674831952,1.16339523992486E-15));
#10895=CARTESIAN_POINT('Ctrl Pts',(42.7247004178212,-30.3901775939692,1.19348975147204E-15));
#10896=CARTESIAN_POINT('Ctrl Pts',(42.7276932514519,-30.2969868069435,1.41803387396094E-15));
#10897=CARTESIAN_POINT('Ctrl Pts',(42.7258764989753,-30.2037315753923,-4.64215791567553E-16));
#10898=CARTESIAN_POINT('Ctrl Pts',(42.7193892630461,-30.1107870263199,9.71445146547012E-17));
#10899=CARTESIAN_POINT('Ctrl Pts',(42.7128890684809,-30.0176568150351,6.59626171160253E-16));
#10900=CARTESIAN_POINT('Ctrl Pts',(42.7016993292407,-29.9248375470543,-1.8032818589036E-15));
#10901=CARTESIAN_POINT('Ctrl Pts',(42.6859089377377,-29.8327186037965,-2.88657986402541E-15));
#10902=CARTESIAN_POINT('Ctrl Pts',(42.6703416524813,-29.7419012312863,-3.95457169058614E-15));
#10903=CARTESIAN_POINT('Ctrl Pts',(42.6503023361097,-29.651763686107,1.83421046840484E-15));
#10904=CARTESIAN_POINT('Ctrl Pts',(42.6258331190092,-29.5627042281559,2.1094237467878E-15));
#10905=CARTESIAN_POINT('Ctrl Pts',(42.6163194528175,-29.5280777850343,2.21642705838946E-15));
#10906=CARTESIAN_POINT('Ctrl Pts',(42.6061357056814,-29.4936146514553,-2.51880313695631E-15));
#10907=CARTESIAN_POINT('Ctrl Pts',(42.5952827870604,-29.4593396971683,-2.66453525910038E-15));
#10908=CARTESIAN_POINT('Ctrl Pts',(42.5894785729062,-29.4410092202016,-2.74247378196201E-15));
#10909=CARTESIAN_POINT('Ctrl Pts',(42.5834829492134,-29.422732581524,4.35205348445305E-15));
#10910=CARTESIAN_POINT('Ctrl Pts',(42.5772959593921,-29.4045136996676,4.52415882534751E-15));
#10911=CARTESIAN_POINT('Ctrl Pts',(42.5718473784623,-29.388469216791,4.6757236259051E-15));
#10912=CARTESIAN_POINT('Ctrl Pts',(42.5662499050538,-29.3724684527645,-1.66194925938346E-15));
#10913=CARTESIAN_POINT('Ctrl Pts',(42.5605096902647,-29.3565304936658,-1.31838984174237E-15));
#10914=CARTESIAN_POINT('Ctrl Pts',(42.5280842271611,-29.2664997676932,6.22316844309968E-16));
#10915=CARTESIAN_POINT('Ctrl Pts',(42.4910677197366,-29.1783477753058,4.42868535318251E-15));
#10916=CARTESIAN_POINT('Ctrl Pts',(42.4495332018698,-29.0925190835637,6.48092690624935E-15));
#10917=CARTESIAN_POINT('Ctrl Pts',(42.4183823134697,-29.0281475647571,8.02010807104948E-15));
#10918=CARTESIAN_POINT('Ctrl Pts',(42.3846888958494,-28.965083439524,2.11771072648854E-15));
#10919=CARTESIAN_POINT('Ctrl Pts',(42.34846639183,-28.9035314164698,3.03229663600746E-15));
#10920=CARTESIAN_POINT('Ctrl Pts',(42.3335346051443,-28.8781581932981,3.40931092799006E-15));
#10921=CARTESIAN_POINT('Ctrl Pts',(42.3181728910835,-28.8530421194055,2.64502491527703E-15));
#10922=CARTESIAN_POINT('Ctrl Pts',(42.3023815334246,-28.8281984400257,2.37310171513627E-15));
#10923=CARTESIAN_POINT('Ctrl Pts',(42.2929488997925,-28.8133585934004,2.21067414061172E-15));
#10924=CARTESIAN_POINT('Ctrl Pts',(42.2833676471414,-28.7986233574288,4.22105548283075E-15));
#10925=CARTESIAN_POINT('Ctrl Pts',(42.2736398143272,-28.7839980537574,3.90659726789977E-15));
#10926=CARTESIAN_POINT('Ctrl Pts',(42.2261111297762,-28.7125410850842,2.37020313084679E-15));
#10927=CARTESIAN_POINT('Ctrl Pts',(42.1750736539845,-28.6436860898129,1.77149268136323E-15));
#10928=CARTESIAN_POINT('Ctrl Pts',(42.1205617687127,-28.5777857785416,2.25514051876985E-16));
#10929=CARTESIAN_POINT('Ctrl Pts',(42.0689757570806,-28.5154226038532,-1.23748564380198E-15));
#10930=CARTESIAN_POINT('Ctrl Pts',(42.014277806743,-28.4557052264058,-1.96483870085748E-15));
#10931=CARTESIAN_POINT('Ctrl Pts',(41.9564732643226,-28.3989684314093,-2.17707796235089E-15));
#10932=CARTESIAN_POINT('Ctrl Pts',(41.9435072914684,-28.3862419619494,-2.23121674702981E-15));
#10933=CARTESIAN_POINT('Ctrl Pts',(41.9303849287496,-28.3736656153915,-2.32254674784139E-15));
#10934=CARTESIAN_POINT('Ctrl Pts',(41.9171094063105,-28.36124072171,-2.27595720048157E-15));
#10935=CARTESIAN_POINT('Ctrl Pts',(37.4805319060517,-30.0019779656107,8.38741669750802));
#10936=CARTESIAN_POINT('Ctrl Pts',(37.4794104066332,-30.1321096319321,8.3956620675864));
#10937=CARTESIAN_POINT('Ctrl Pts',(37.4886219042959,-30.2620820392616,8.40390743766478));
#10938=CARTESIAN_POINT('Ctrl Pts',(37.5087194067633,-30.3903486407411,8.41215280774316));
#10939=CARTESIAN_POINT('Ctrl Pts',(37.6377282224616,-31.2137107663279,8.46508104748506));
#10940=CARTESIAN_POINT('Ctrl Pts',(38.2152996968383,-31.9667844049101,8.51800928722696));
#10941=CARTESIAN_POINT('Ctrl Pts',(38.9770562477556,-32.3048689279236,8.57093752696885));
#10942=CARTESIAN_POINT('Ctrl Pts',(39.7388127986728,-32.6429534509372,8.62386576671074));
#10943=CARTESIAN_POINT('Ctrl Pts',(40.6847544261306,-32.5660488583821,8.67679400645263));
#10944=CARTESIAN_POINT('Ctrl Pts',(41.3818821863494,-32.1093324065798,8.72972224619453));
#10945=CARTESIAN_POINT('Ctrl Pts',(42.0790099465682,-31.6526159547776,8.78265048593643));
#10946=CARTESIAN_POINT('Ctrl Pts',(42.5273238395481,-30.8160876437281,8.83557872567832));
#10947=CARTESIAN_POINT('Ctrl Pts',(42.5216158322499,-29.9827117038109,8.88850696542022));
#10948=CARTESIAN_POINT('Ctrl Pts',(42.5159078249518,-29.1493357638938,8.94143520516211));
#10949=CARTESIAN_POINT('Ctrl Pts',(42.0561779173756,-28.3191121951089,8.994363444904));
#10950=CARTESIAN_POINT('Ctrl Pts',(41.3528557911673,-27.8719684989796,9.0472916846459));
#10951=CARTESIAN_POINT('Ctrl Pts',(40.6495336649589,-27.4248248028504,9.10021992438779));
#10952=CARTESIAN_POINT('Ctrl Pts',(39.7026193201184,-27.3607609793766,9.15314816412968));
#10953=CARTESIAN_POINT('Ctrl Pts',(38.9455707232652,-27.709302425205,9.20607640387158));
#10954=CARTESIAN_POINT('Ctrl Pts',(38.1885221264121,-28.0578438710333,9.25900464361348));
#10955=CARTESIAN_POINT('Ctrl Pts',(37.6213392775464,-28.8189905861637,9.31193288335538));
#10956=CARTESIAN_POINT('Ctrl Pts',(37.5036140624373,-29.6439328598341,9.36486112309727));
#10957=CARTESIAN_POINT('Ctrl Pts',(37.486891043608,-29.7611169750883,9.37237964790086));
#10958=CARTESIAN_POINT('Ctrl Pts',(37.4792374368207,-29.8795883934461,9.37989817270444));
#10959=CARTESIAN_POINT('Ctrl Pts',(37.4802181636634,-29.9981833349058,9.38741669750803));
#10960=CARTESIAN_POINT('Ctrl Pts',(39.2062007174671,-32.9692229537457,10.));
#10961=CARTESIAN_POINT('Ctrl Pts',(38.2187620536724,-32.7052387009375,9.94707176025811));
#10962=CARTESIAN_POINT('Ctrl Pts',(36.5451692871586,-31.1184273543511,9.84121528077431));
#10963=CARTESIAN_POINT('Ctrl Pts',(37.1870307188556,-27.697626748216,9.68243056154864));
#10964=CARTESIAN_POINT('Ctrl Pts',(40.4091142364954,-26.3909769590634,9.52364584232295));
#10965=CARTESIAN_POINT('Ctrl Pts',(43.2541892892138,-28.3852504471766,9.36486112309727));
#10966=CARTESIAN_POINT('Ctrl Pts',(43.1213433300866,-31.8593327642316,9.20607640387157));
#10967=CARTESIAN_POINT('Ctrl Pts',(40.1303404283627,-33.6304598448459,9.04729168464591));
#10968=CARTESIAN_POINT('Ctrl Pts',(37.0203228967143,-32.0783449395581,8.88850696542022));
#10969=CARTESIAN_POINT('Ctrl Pts',(36.6379953175286,-28.6233472228274,8.72972224619453));
#10970=CARTESIAN_POINT('Ctrl Pts',(39.3336052322159,-26.4287487288557,8.57093752696886));
#10971=CARTESIAN_POINT('Ctrl Pts',(42.6392496071423,-27.5035235206868,8.41215280774315));
#10972=CARTESIAN_POINT('Ctrl Pts',(43.5287240702543,-30.8638054618116,8.25336808851749));
#10973=CARTESIAN_POINT('Ctrl Pts',(41.1877001687398,-33.4332756644217,8.09458336929179));
#10974=CARTESIAN_POINT('Ctrl Pts',(37.7593612762403,-32.8596447757211,7.93579865006612));
#10975=CARTESIAN_POINT('Ctrl Pts',(36.3822876706404,-29.6680532961916,7.77701393084043));
#10976=CARTESIAN_POINT('Ctrl Pts',(38.3171711686706,-26.7803550620374,7.61822921161474));
#10977=CARTESIAN_POINT('Ctrl Pts',(41.7926560478477,-26.8401878205589,7.45944449238907));
#10978=CARTESIAN_POINT('Ctrl Pts',(43.6269942364715,-29.7927768135681,7.30065977316338));
#10979=CARTESIAN_POINT('Ctrl Pts',(42.1408789623084,-32.935075019391,7.1418750539377));
#10980=CARTESIAN_POINT('Ctrl Pts',(38.6948244410116,-33.3903606257847,6.98309033471201));
#10981=CARTESIAN_POINT('Ctrl Pts',(36.4436365448214,-30.7418270372989,6.82430561548633));
#10982=CARTESIAN_POINT('Ctrl Pts',(37.4482406630067,-27.4141630745731,6.66552089626065));
#10983=CARTESIAN_POINT('Ctrl Pts',(40.7889382915105,-26.453790089119,6.50673617703496));
#10984=CARTESIAN_POINT('Ctrl Pts',(43.4073759516192,-28.7399137026036,6.34795145780928));
#10985=CARTESIAN_POINT('Ctrl Pts',(42.9064172126614,-32.1796255027351,6.18916673858359));
#10986=CARTESIAN_POINT('Ctrl Pts',(39.7446815283789,-33.6239261622643,6.03038201935791));
#10987=CARTESIAN_POINT('Ctrl Pts',(36.816685686601,-31.7505822837933,5.87159730013222));
#10988=CARTESIAN_POINT('Ctrl Pts',(36.8029615132848,-28.2746092430835,5.71281258090655));
#10989=CARTESIAN_POINT('Ctrl Pts',(39.7160732619294,-26.3782029380897,5.55402786168086));
#10990=CARTESIAN_POINT('Ctrl Pts',(42.8891152491159,-27.7974920142308,5.39524314245518));
#10991=CARTESIAN_POINT('Ctrl Pts',(43.4172199515306,-31.2331407676563,5.2364584232295));
#10992=CARTESIAN_POINT('Ctrl Pts',(40.8169162380303,-33.5398695187991,5.07767370400381));
#10993=CARTESIAN_POINT('Ctrl Pts',(37.4687392033951,-32.6059062012305,4.91888898477812));
#10994=CARTESIAN_POINT('Ctrl Pts',(36.4378896136882,-29.2862788038946,4.76010426555244));
#10995=CARTESIAN_POINT('Ctrl Pts',(38.6680932394838,-26.6200513714892,4.60131954632676));
#10996=CARTESIAN_POINT('Ctrl Pts',(42.1176355025165,-27.0481110745022,4.44253482710108));
#10997=CARTESIAN_POINT('Ctrl Pts',(43.6285174446119,-30.1785763259747,4.28375010787539));
#10998=CARTESIAN_POINT('Ctrl Pts',(41.8175516063153,-33.1455579010144,4.12496538864971));
#10999=CARTESIAN_POINT('Ctrl Pts',(38.3426472969195,-33.2328331796093,3.96618066942402));
#11000=CARTESIAN_POINT('Ctrl Pts',(36.3850220090575,-30.3605030862883,3.80739595019834));
#11001=CARTESIAN_POINT('Ctrl Pts',(37.7368493554468,-27.1581383722016,3.64861123097266));
#11002=CARTESIAN_POINT('Ctrl Pts',(41.1605537314434,-26.5574510340941,3.48982651174697));
#11003=CARTESIAN_POINT('Ctrl Pts',(43.5217903378555,-29.1083604042289,3.33104179252129));
#11004=CARTESIAN_POINT('Ctrl Pts',(42.6588860667731,-32.4755510990005,3.17225707329561));
#11005=CARTESIAN_POINT('Ctrl Pts',(39.3618155247875,-33.5764156490026,3.01347235406992));
#11006=CARTESIAN_POINT('Ctrl Pts',(36.6489923263848,-31.4031307672381,2.85468763484424));
#11007=CARTESIAN_POINT('Ctrl Pts',(37.0039612996256,-27.9453028158605,2.69590291561856));
#11008=CARTESIAN_POINT('Ctrl Pts',(40.1017542062109,-26.3685162560978,2.53711819639287));
#11009=CARTESIAN_POINT('Ctrl Pts',(43.1063928273453,-28.1162929520197,2.37833347716719));
#11010=CARTESIAN_POINT('Ctrl Pts',(43.2671801112825,-31.58857257803,2.2195487579415));
#11011=CARTESIAN_POINT('Ctrl Pts',(40.4369180121167,-33.6065397617092,2.06076403871582));
#11012=CARTESIAN_POINT('Ctrl Pts',(37.2066646152815,-32.3227803470516,1.90197931949014));
#11013=CARTESIAN_POINT('Ctrl Pts',(36.5336637694756,-28.9125519457581,1.74319460026446));
#11014=CARTESIAN_POINT('Ctrl Pts',(39.034036182301,-26.4978681661549,1.58440988103877));
#11015=CARTESIAN_POINT('Ctrl Pts',(42.4187331109537,-27.2893204582939,1.42562516181309));
#11016=CARTESIAN_POINT('Ctrl Pts',(43.5891186388302,-30.5623706046428,1.26684044258741));
#11017=CARTESIAN_POINT('Ctrl Pts',(41.4737277243454,-33.3205487833603,1.10805572336172));
#11018=CARTESIAN_POINT('Ctrl Pts',(38.0091586671154,-33.0388812318245,0.949271004136037));
#11019=CARTESIAN_POINT('Ctrl Pts',(36.3671814579584,-29.9750446753109,0.790486284910354));
#11020=CARTESIAN_POINT('Ctrl Pts',(38.0509706569457,-26.9343007433511,0.63170156568467));
#11021=CARTESIAN_POINT('Ctrl Pts',(41.5191018646847,-26.6996618298828,0.472916846458986));
#11022=CARTESIAN_POINT('Ctrl Pts',(43.5964448997665,-29.4874103675251,0.314132127233304));
#11023=CARTESIAN_POINT('Ctrl Pts',(42.3814522873891,-32.7424636317378,0.155347408007619));
#11024=CARTESIAN_POINT('Ctrl Pts',(38.9859863107926,-33.4907728378243,-0.00343731121806265));
#11025=CARTESIAN_POINT('Ctrl Pts',(36.5193436061198,-31.0352613530379,-0.162222030443749));
#11026=CARTESIAN_POINT('Ctrl Pts',(36.9997188544053,-28.7795746242084,-0.268078509927537));
#11027=CARTESIAN_POINT('Ctrl Pts',(37.6639373423039,-28.0026984430693,-0.321006749669432));
#11028=CARTESIAN_POINT('Ctrl Pts',(39.254067145653,-32.7901775698422,10.1070022498898));
#11029=CARTESIAN_POINT('Ctrl Pts',(38.326171445588,-32.5421116777044,10.0540740101479));
#11030=CARTESIAN_POINT('Ctrl Pts',(36.7534970217,-31.0509857178868,9.94821753066413));
#11031=CARTESIAN_POINT('Ctrl Pts',(37.3566539410579,-27.8364608166496,9.78943281143844));
#11032=CARTESIAN_POINT('Ctrl Pts',(40.3844444772099,-26.6086025553717,9.63064809221276));
#11033=CARTESIAN_POINT('Ctrl Pts',(43.0579603162945,-28.4826205194471,9.47186337298708));
#11034=CARTESIAN_POINT('Ctrl Pts',(42.9331250239721,-31.747214222188,9.31307865376139));
#11035=CARTESIAN_POINT('Ctrl Pts',(40.1224808461091,-33.411541600311,9.15429393453572));
#11036=CARTESIAN_POINT('Ctrl Pts',(37.1999986702002,-31.9530198718943,8.99550921531002));
#11037=CARTESIAN_POINT('Ctrl Pts',(36.8407256036794,-28.7063599601093,8.83672449608434));
#11038=CARTESIAN_POINT('Ctrl Pts',(39.373789114965,-26.644096671674,8.67793977685866));
#11039=CARTESIAN_POINT('Ctrl Pts',(42.4801017538186,-27.6540620947878,8.51915505763297));
#11040=CARTESIAN_POINT('Ctrl Pts',(43.3159405354069,-30.8117176317842,8.36037033840729));
#11041=CARTESIAN_POINT('Ctrl Pts',(41.1160813526431,-33.2262477083002,8.2015856191816));
#11042=CARTESIAN_POINT('Ctrl Pts',(37.8944727268569,-32.6872070017066,8.04280089995594));
#11043=CARTESIAN_POINT('Ctrl Pts',(36.6004372346688,-29.6880698210349,7.88401618073023));
#11044=CARTESIAN_POINT('Ctrl Pts',(38.4186464498613,-26.9745009961524,7.72523146150456));
#11045=CARTESIAN_POINT('Ctrl Pts',(41.6845581396429,-27.030725814352,7.56644674227887));
#11046=CARTESIAN_POINT('Ctrl Pts',(43.4082849695686,-29.8052724582355,7.40766202305319));
#11047=CARTESIAN_POINT('Ctrl Pts',(42.0117830669618,-32.7580887701874,7.24887730382751));
#11048=CARTESIAN_POINT('Ctrl Pts',(38.7735270721919,-33.185920464412,7.09009258460182));
#11049=CARTESIAN_POINT('Ctrl Pts',(36.6580867461206,-30.6970945572015,6.93130786537614));
#11050=CARTESIAN_POINT('Ctrl Pts',(37.6021128165091,-27.570090120887,6.77252314615045));
#11051=CARTESIAN_POINT('Ctrl Pts',(40.7413649831129,-26.6676280274574,6.61373842692477));
#11052=CARTESIAN_POINT('Ctrl Pts',(43.2019097589942,-28.815897432483,6.45495370769909));
#11053=CARTESIAN_POINT('Ctrl Pts',(42.7311590411695,-32.0481931748222,6.29616898847341));
#11054=CARTESIAN_POINT('Ctrl Pts',(39.7600773388253,-33.4054019015172,6.13738426924772));
#11055=CARTESIAN_POINT('Ctrl Pts',(37.0086408688851,-31.6450214411286,5.97859955002204));
#11056=CARTESIAN_POINT('Ctrl Pts',(36.9957442689502,-28.3786510261588,5.81981483079635));
#11057=CARTESIAN_POINT('Ctrl Pts',(39.7331941627881,-26.5965988131964,5.66103011157067));
#11058=CARTESIAN_POINT('Ctrl Pts',(42.7149003932503,-27.9303041654252,5.50224539234499));
#11059=CARTESIAN_POINT('Ctrl Pts',(43.2111601616005,-31.1587818644713,5.3434606731193));
#11060=CARTESIAN_POINT('Ctrl Pts',(40.7676558477754,-33.3264139087506,5.18467595389362));
#11061=CARTESIAN_POINT('Ctrl Pts',(37.6213752863529,-32.4487689692057,5.02589123466793));
#11062=CARTESIAN_POINT('Ctrl Pts',(36.6526863573343,-29.3293164900325,4.86710651544226));
#11063=CARTESIAN_POINT('Ctrl Pts',(38.7484077732778,-26.8238636850788,4.70832179621656));
#11064=CARTESIAN_POINT('Ctrl Pts',(41.9899411975006,-27.2261112092646,4.54953707699089));
#11065=CARTESIAN_POINT('Ctrl Pts',(43.4097163276221,-30.1678080989543,4.3907523577652));
#11066=CARTESIAN_POINT('Ctrl Pts',(41.7079524855398,-32.9558794461623,4.23196763853952));
#11067=CARTESIAN_POINT('Ctrl Pts',(38.4425863569393,-33.0378919890163,4.07318291931383));
#11068=CARTESIAN_POINT('Ctrl Pts',(36.6030066913377,-30.3387645996578,3.91439820008815));
#11069=CARTESIAN_POINT('Ctrl Pts',(37.8733182842871,-27.329503814971,3.75561348086247));
#11070=CARTESIAN_POINT('Ctrl Pts',(41.0905718568507,-26.7650381741672,3.59682876163679));
#11071=CARTESIAN_POINT('Ctrl Pts',(43.3094249099668,-29.1621266441561,3.4380440424111));
#11072=CARTESIAN_POINT('Ctrl Pts',(42.4985541267346,-32.3262743340697,3.27925932318542));
#11073=CARTESIAN_POINT('Ctrl Pts',(39.4002983151154,-33.3607562920431,3.12047460395974));
#11074=CARTESIAN_POINT('Ctrl Pts',(36.8510594883099,-31.3185213960994,2.96168988473405));
#11075=CARTESIAN_POINT('Ctrl Pts',(37.1846236842477,-28.0692019139985,2.80290516550837));
#11076=CARTESIAN_POINT('Ctrl Pts',(40.0956183850892,-26.5874962421734,2.64412044628268));
#11077=CARTESIAN_POINT('Ctrl Pts',(42.9190760427886,-28.2298812735507,2.485335727057));
#11078=CARTESIAN_POINT('Ctrl Pts',(43.0701677863682,-31.4927809882697,2.32655100783132));
#11079=CARTESIAN_POINT('Ctrl Pts',(40.4105716735518,-33.3890639081753,2.16776628860563));
#11080=CARTESIAN_POINT('Ctrl Pts',(37.3751039053313,-32.1827157222525,2.00898156937995));
#11081=CARTESIAN_POINT('Ctrl Pts',(36.7426852915375,-28.9781255174905,1.85019685015427));
#11082=CARTESIAN_POINT('Ctrl Pts',(39.0922842038443,-26.7090481780434,1.69141213092858));
#11083=CARTESIAN_POINT('Ctrl Pts',(42.2728824944264,-27.4527755664972,1.5326274117029));
#11084=CARTESIAN_POINT('Ctrl Pts',(43.3726932862799,-30.5284594223662,1.37384269247721));
#11085=CARTESIAN_POINT('Ctrl Pts',(41.3848613272155,-33.1203183052356,1.21505797325153));
#11086=CARTESIAN_POINT('Ctrl Pts',(38.1292072307599,-32.8556354246672,1.05627325402585));
#11087=CARTESIAN_POINT('Ctrl Pts',(36.5862419329191,-29.9765494918096,0.897488534800165));
#11088=CARTESIAN_POINT('Ctrl Pts',(38.1684979401449,-27.1191636886031,0.73870381557448));
#11089=CARTESIAN_POINT('Ctrl Pts',(41.4274993879465,-26.8986735995899,0.579919096348797));
#11090=CARTESIAN_POINT('Ctrl Pts',(43.3795777706227,-29.518319736394,0.421134377123114));
#11091=CARTESIAN_POINT('Ctrl Pts',(42.2378497200892,-32.5770919296341,0.26234965789743));
#11092=CARTESIAN_POINT('Ctrl Pts',(39.0471317596511,-33.2802777781389,0.103564938671748));
#11093=CARTESIAN_POINT('Ctrl Pts',(36.7292286400114,-30.9728346611785,-0.0552197805539377));
#11094=CARTESIAN_POINT('Ctrl Pts',(37.1806370602456,-28.8531667839546,-0.161076260037726));
#11095=CARTESIAN_POINT('Ctrl Pts',(37.8048028959809,-28.1231365609212,-0.214004499779622));
#11096=CARTESIAN_POINT('Ctrl Pts',(39.301933573839,-32.6111321859386,10.2140044997796));
#11097=CARTESIAN_POINT('Ctrl Pts',(38.4335808375037,-32.3789846544712,10.1610762600377));
#11098=CARTESIAN_POINT('Ctrl Pts',(36.9618247562416,-30.9835440814225,10.0552197805539));
#11099=CARTESIAN_POINT('Ctrl Pts',(37.5262771632602,-27.9752948850832,9.89643506132825));
#11100=CARTESIAN_POINT('Ctrl Pts',(40.3597747179245,-26.82622815168,9.73765034210258));
#11101=CARTESIAN_POINT('Ctrl Pts',(42.8617313433752,-28.5799905917176,9.57886562287688));
#11102=CARTESIAN_POINT('Ctrl Pts',(42.7449067178577,-31.6350956801444,9.42008090365121));
#11103=CARTESIAN_POINT('Ctrl Pts',(40.1146212638554,-33.1926233557761,9.26129618442551));
#11104=CARTESIAN_POINT('Ctrl Pts',(37.3796744436861,-31.8276948042305,9.10251146519985));
#11105=CARTESIAN_POINT('Ctrl Pts',(37.0434558898303,-28.7893726973912,8.94372674597414));
#11106=CARTESIAN_POINT('Ctrl Pts',(39.4139729977141,-26.8594446144923,8.78494202674848));
#11107=CARTESIAN_POINT('Ctrl Pts',(42.3209539004949,-27.8046006688888,8.62615730752278));
#11108=CARTESIAN_POINT('Ctrl Pts',(43.1031570005594,-30.7596298017569,8.46737258829711));
#11109=CARTESIAN_POINT('Ctrl Pts',(41.0444625365464,-33.0192197521787,8.30858786907141));
#11110=CARTESIAN_POINT('Ctrl Pts',(38.0295841774735,-32.514769227692,8.14980314984574));
#11111=CARTESIAN_POINT('Ctrl Pts',(36.8185867986972,-29.7080863458782,7.99101843062005));
#11112=CARTESIAN_POINT('Ctrl Pts',(38.5201217310521,-27.1686469302674,7.83223371139437));
#11113=CARTESIAN_POINT('Ctrl Pts',(41.5764602314379,-27.2212638081451,7.67344899216869));
#11114=CARTESIAN_POINT('Ctrl Pts',(43.1895757026657,-29.817768102903,7.514664272943));
#11115=CARTESIAN_POINT('Ctrl Pts',(41.8826871716151,-32.5811025209839,7.35587955371732));
#11116=CARTESIAN_POINT('Ctrl Pts',(38.8522297033722,-32.9814803030395,7.19709483449163));
#11117=CARTESIAN_POINT('Ctrl Pts',(36.8725369474198,-30.652362077104,7.03831011526595));
#11118=CARTESIAN_POINT('Ctrl Pts',(37.7559849700114,-27.726017167201,6.87952539604027));
#11119=CARTESIAN_POINT('Ctrl Pts',(40.6937916747153,-26.8814659657959,6.72074067681458));
#11120=CARTESIAN_POINT('Ctrl Pts',(42.996443566369,-28.8918811623623,6.56195595758891));
#11121=CARTESIAN_POINT('Ctrl Pts',(42.5559008696777,-31.9167608469093,6.40317123836321));
#11122=CARTESIAN_POINT('Ctrl Pts',(39.7754731492718,-33.18687764077,6.24438651913754));
#11123=CARTESIAN_POINT('Ctrl Pts',(37.200596051169,-31.539460598464,6.08560179991185));
#11124=CARTESIAN_POINT('Ctrl Pts',(37.1885270246158,-28.4826928092341,5.92681708068617));
#11125=CARTESIAN_POINT('Ctrl Pts',(39.7503150636467,-26.8149946883032,5.76803236146048));
#11126=CARTESIAN_POINT('Ctrl Pts',(42.5406855373847,-28.0631163166195,5.6092476422348));
#11127=CARTESIAN_POINT('Ctrl Pts',(43.0051003716703,-31.0844229612864,5.45046292300912));
#11128=CARTESIAN_POINT('Ctrl Pts',(40.7183954575206,-33.112958298702,5.29167820378343));
#11129=CARTESIAN_POINT('Ctrl Pts',(37.7740113693106,-32.291631737181,5.13289348455775));
#11130=CARTESIAN_POINT('Ctrl Pts',(36.8674831009805,-29.3723541761704,4.97410876533207));
#11131=CARTESIAN_POINT('Ctrl Pts',(38.8287223070717,-27.0276759986683,4.81532404610638));
#11132=CARTESIAN_POINT('Ctrl Pts',(41.8622468924847,-27.404111344027,4.6565393268807));
#11133=CARTESIAN_POINT('Ctrl Pts',(43.1909152106323,-30.1570398719339,4.49775460765501));
#11134=CARTESIAN_POINT('Ctrl Pts',(41.5983533647642,-32.7662009913101,4.33896988842933));
#11135=CARTESIAN_POINT('Ctrl Pts',(38.5425254169591,-32.8429507984234,4.18018516920365));
#11136=CARTESIAN_POINT('Ctrl Pts',(36.8209913736178,-30.3170261130273,4.02140044997796));
#11137=CARTESIAN_POINT('Ctrl Pts',(38.0097872131274,-27.5008692577405,3.86261573075228));
#11138=CARTESIAN_POINT('Ctrl Pts',(41.0205899822579,-26.9726253142402,3.7038310115266));
#11139=CARTESIAN_POINT('Ctrl Pts',(43.0970594820782,-29.2158928840833,3.54504629230091));
#11140=CARTESIAN_POINT('Ctrl Pts',(42.3382221866959,-32.1769975691389,3.38626157307523));
#11141=CARTESIAN_POINT('Ctrl Pts',(39.4387811054433,-33.1450969350836,3.22747685384954));
#11142=CARTESIAN_POINT('Ctrl Pts',(37.0531266502349,-31.2339120249606,3.06869213462386));
#11143=CARTESIAN_POINT('Ctrl Pts',(37.3652860688698,-28.1931010121365,2.90990741539817));
#11144=CARTESIAN_POINT('Ctrl Pts',(40.0894825639675,-26.8064762282489,2.7511226961725));
#11145=CARTESIAN_POINT('Ctrl Pts',(42.7317592582321,-28.3434695950818,2.59233797694681));
#11146=CARTESIAN_POINT('Ctrl Pts',(42.8731554614538,-31.3969893985094,2.43355325772113));
#11147=CARTESIAN_POINT('Ctrl Pts',(40.384225334987,-33.1715880546413,2.27476853849545));
#11148=CARTESIAN_POINT('Ctrl Pts',(37.543543195381,-32.0426510974533,2.11598381926976));
#11149=CARTESIAN_POINT('Ctrl Pts',(36.9517068135993,-29.0436990892229,1.95719910004408));
#11150=CARTESIAN_POINT('Ctrl Pts',(39.1505322253877,-26.9202281899319,1.79841438081839));
#11151=CARTESIAN_POINT('Ctrl Pts',(42.1270318778991,-27.6162306747005,1.63962966159271));
#11152=CARTESIAN_POINT('Ctrl Pts',(43.1562679337296,-30.4945482400896,1.48084494236703));
#11153=CARTESIAN_POINT('Ctrl Pts',(41.2959949300857,-32.920087827111,1.32206022314134));
#11154=CARTESIAN_POINT('Ctrl Pts',(38.2492557944043,-32.6723896175098,1.16327550391566));
#11155=CARTESIAN_POINT('Ctrl Pts',(36.8053024078799,-29.9780543083085,1.00449078468998));
#11156=CARTESIAN_POINT('Ctrl Pts',(38.286025223344,-27.3040266338552,0.845706065464291));
#11157=CARTESIAN_POINT('Ctrl Pts',(41.3358969112083,-27.0976853692971,0.686921346238607));
#11158=CARTESIAN_POINT('Ctrl Pts',(43.1627106414789,-29.549229105263,0.528136627012926));
#11159=CARTESIAN_POINT('Ctrl Pts',(42.0942471527894,-32.4117202275306,0.36935190778724));
#11160=CARTESIAN_POINT('Ctrl Pts',(39.1082772085095,-33.0697827184533,0.210567188561559));
#11161=CARTESIAN_POINT('Ctrl Pts',(36.939113673903,-30.9104079693192,0.0517824693358731));
#11162=CARTESIAN_POINT('Ctrl Pts',(37.3615552660859,-28.9267589437008,-0.0540740101479155));
#11163=CARTESIAN_POINT('Ctrl Pts',(37.9456684496579,-28.2435746787731,-0.107002249889811));
#11164=CARTESIAN_POINT('Ctrl Pts',(39.3498000020249,-32.4320868020351,10.3210067496694));
#11165=CARTESIAN_POINT('Ctrl Pts',(38.5409902294193,-32.2158576312381,10.2680785099275));
#11166=CARTESIAN_POINT('Ctrl Pts',(37.170152490783,-30.9161024449581,10.1622220304438));
#11167=CARTESIAN_POINT('Ctrl Pts',(37.6959003854625,-28.1141289535168,10.0034373112181));
#11168=CARTESIAN_POINT('Ctrl Pts',(40.335104958639,-27.0438537479883,9.84465259199239));
#11169=CARTESIAN_POINT('Ctrl Pts',(42.6655023704558,-28.6773606639881,9.6858678727667));
#11170=CARTESIAN_POINT('Ctrl Pts',(42.5566884117433,-31.5229771381009,9.52708315354101));
#11171=CARTESIAN_POINT('Ctrl Pts',(40.1067616816018,-32.9737051112411,9.36829843431534));
#11172=CARTESIAN_POINT('Ctrl Pts',(37.559350217172,-31.7023697365666,9.20951371508965));
#11173=CARTESIAN_POINT('Ctrl Pts',(37.2461861759812,-28.8723854346731,9.05072899586396));
#11174=CARTESIAN_POINT('Ctrl Pts',(39.4541568804632,-27.0747925573107,8.89194427663828));
#11175=CARTESIAN_POINT('Ctrl Pts',(42.1618060471712,-27.9551392429898,8.7331595574126));
#11176=CARTESIAN_POINT('Ctrl Pts',(42.8903734657118,-30.7075419717295,8.57437483818692));
#11177=CARTESIAN_POINT('Ctrl Pts',(40.9728437204498,-32.8121917960571,8.41559011896122));
#11178=CARTESIAN_POINT('Ctrl Pts',(38.1646956280901,-32.3423314536776,8.25680539973556));
#11179=CARTESIAN_POINT('Ctrl Pts',(37.0367363627256,-29.7281028707214,8.09802068050985));
#11180=CARTESIAN_POINT('Ctrl Pts',(38.6215970122427,-27.3627928643824,7.93923596128418));
#11181=CARTESIAN_POINT('Ctrl Pts',(41.468362323233,-27.4118018019382,7.7804512420585));
#11182=CARTESIAN_POINT('Ctrl Pts',(42.9708664357628,-29.8302637475704,7.62166652283281));
#11183=CARTESIAN_POINT('Ctrl Pts',(41.7535912762685,-32.4041162717803,7.46288180360713));
#11184=CARTESIAN_POINT('Ctrl Pts',(38.9309323345525,-32.7770401416668,7.30409708438144));
#11185=CARTESIAN_POINT('Ctrl Pts',(37.0869871487189,-30.6076295970066,7.14531236515576));
#11186=CARTESIAN_POINT('Ctrl Pts',(37.9098571235138,-27.8819442135148,6.98652764593008));
#11187=CARTESIAN_POINT('Ctrl Pts',(40.6462183663177,-27.0953039041344,6.82774292670439));
#11188=CARTESIAN_POINT('Ctrl Pts',(42.7909773737438,-28.9678648922416,6.66895820747872));
#11189=CARTESIAN_POINT('Ctrl Pts',(42.3806426981861,-31.7853285189965,6.51017348825302));
#11190=CARTESIAN_POINT('Ctrl Pts',(39.7908689597182,-32.9683533800229,6.35138876902734));
#11191=CARTESIAN_POINT('Ctrl Pts',(37.3925512334531,-31.4338997557994,6.19260404980166));
#11192=CARTESIAN_POINT('Ctrl Pts',(37.3813097802812,-28.5867345923093,6.03381933057598));
#11193=CARTESIAN_POINT('Ctrl Pts',(39.7674359645054,-27.03339056341,5.87503461135029));
#11194=CARTESIAN_POINT('Ctrl Pts',(42.3664706815192,-28.1959284678139,5.71624989212461));
#11195=CARTESIAN_POINT('Ctrl Pts',(42.7990405817402,-31.0100640581014,5.55746517289893));
#11196=CARTESIAN_POINT('Ctrl Pts',(40.6691350672658,-32.8995026886535,5.39868045367324));
#11197=CARTESIAN_POINT('Ctrl Pts',(37.9266474522684,-32.1344945051563,5.23989573444756));
#11198=CARTESIAN_POINT('Ctrl Pts',(37.0822798446267,-29.4153918623083,5.08111101522188));
#11199=CARTESIAN_POINT('Ctrl Pts',(38.9090368408656,-27.2314883122577,4.92232629599619));
#11200=CARTESIAN_POINT('Ctrl Pts',(41.7345525874688,-27.5821114787895,4.76354157677051));
#11201=CARTESIAN_POINT('Ctrl Pts',(42.9721140936425,-30.1462716449134,4.60475685754482));
#11202=CARTESIAN_POINT('Ctrl Pts',(41.4887542439886,-32.576522536458,4.44597213831914));
#11203=CARTESIAN_POINT('Ctrl Pts',(38.6424644769789,-32.6480096078303,4.28718741909346));
#11204=CARTESIAN_POINT('Ctrl Pts',(37.038976055898,-30.2952876263969,4.12840269986778));
#11205=CARTESIAN_POINT('Ctrl Pts',(38.1462561419676,-27.67223470051,3.96961798064208));
#11206=CARTESIAN_POINT('Ctrl Pts',(40.9506081076652,-27.1802124543133,3.81083326141641));
#11207=CARTESIAN_POINT('Ctrl Pts',(42.8846940541895,-29.2696591240105,3.65204854219072));
#11208=CARTESIAN_POINT('Ctrl Pts',(42.1778902466573,-32.0277208042081,3.49326382296504));
#11209=CARTESIAN_POINT('Ctrl Pts',(39.4772638957712,-32.929437578124,3.33447910373935));
#11210=CARTESIAN_POINT('Ctrl Pts',(37.25519381216,-31.149302653822,3.17569438451368));
#11211=CARTESIAN_POINT('Ctrl Pts',(37.5459484534919,-28.3170001102745,3.01690966528798));
#11212=CARTESIAN_POINT('Ctrl Pts',(40.0833467428457,-27.0254562143245,2.85812494606231));
#11213=CARTESIAN_POINT('Ctrl Pts',(42.5444424736755,-28.4570579166128,2.69934022683662));
#11214=CARTESIAN_POINT('Ctrl Pts',(42.6761431365394,-31.3011978087492,2.54055550761094));
#11215=CARTESIAN_POINT('Ctrl Pts',(40.3578789964222,-32.9541122011072,2.38177078838526));
#11216=CARTESIAN_POINT('Ctrl Pts',(37.7119824854307,-31.9025864726542,2.22298606915957));
#11217=CARTESIAN_POINT('Ctrl Pts',(37.1607283356612,-29.1092726609553,2.06420134993389));
#11218=CARTESIAN_POINT('Ctrl Pts',(39.208780246931,-27.1314082018204,1.9054166307082));
#11219=CARTESIAN_POINT('Ctrl Pts',(41.9811812613717,-27.7796857829038,1.74663191148252));
#11220=CARTESIAN_POINT('Ctrl Pts',(42.9398425811794,-30.460637057813,1.58784719225683));
#11221=CARTESIAN_POINT('Ctrl Pts',(41.2071285329557,-32.7198573489864,1.42906247303115));
#11222=CARTESIAN_POINT('Ctrl Pts',(38.3693043580489,-32.4891438103524,1.27027775380547));
#11223=CARTESIAN_POINT('Ctrl Pts',(37.0243628828405,-29.9795591248073,1.11149303457979));
#11224=CARTESIAN_POINT('Ctrl Pts',(38.4035525065433,-27.4888895791073,0.952708315354101));
#11225=CARTESIAN_POINT('Ctrl Pts',(41.24429443447,-27.2966971390043,0.793923596128418));
#11226=CARTESIAN_POINT('Ctrl Pts',(42.9458435123352,-29.5801384741319,0.635138876902737));
#11227=CARTESIAN_POINT('Ctrl Pts',(41.9506445854895,-32.246348525427,0.476354157677051));
#11228=CARTESIAN_POINT('Ctrl Pts',(39.169422657368,-32.8592876587678,0.31756943845137));
#11229=CARTESIAN_POINT('Ctrl Pts',(37.1489987077945,-30.8479812774599,0.158784719225684));
#11230=CARTESIAN_POINT('Ctrl Pts',(37.5424734719262,-29.0003511034471,0.0529282397418953));
#11231=CARTESIAN_POINT('Ctrl Pts',(38.0865340033349,-28.364012796625,0.));
#11232=CARTESIAN_POINT('Ctrl Pts',(38.0865340033349,-28.364012796625,5.55111512312578E-17));
#11233=CARTESIAN_POINT('Ctrl Pts',(38.0249211430992,-28.421913756063,2.3104639589866E-16));
#11234=CARTESIAN_POINT('Ctrl Pts',(37.9666794538551,-28.482965221658,1.28255707534279E-15));
#11235=CARTESIAN_POINT('Ctrl Pts',(37.9118058265048,-28.5467823968405,9.43689570931383E-16));
#11236=CARTESIAN_POINT('Ctrl Pts',(37.8554795264063,-28.6122890078363,5.95851207244836E-16));
#11237=CARTESIAN_POINT('Ctrl Pts',(37.8027015385178,-28.6807101321021,2.62784299857289E-16));
#11238=CARTESIAN_POINT('Ctrl Pts',(37.753494049528,-28.7516781506113,6.10622663543836E-16));
#11239=CARTESIAN_POINT('Ctrl Pts',(37.7025923854307,-28.8250895421285,9.7043682825834E-16));
#11240=CARTESIAN_POINT('Ctrl Pts',(37.6555107288522,-28.9012267438899,2.71054820682649E-15));
#11241=CARTESIAN_POINT('Ctrl Pts',(37.6123085670218,-28.9797268371754,2.99760216648792E-15));
#11242=CARTESIAN_POINT('Ctrl Pts',(37.593407621221,-29.0140706279878,3.1231882738398E-15));
#11243=CARTESIAN_POINT('Ctrl Pts',(37.5752497289795,-29.0488671972833,4.75485736688032E-16));
#11244=CARTESIAN_POINT('Ctrl Pts',(37.5578423170003,-29.0840882429965,4.44089209850063E-16));
#11245=CARTESIAN_POINT('Ctrl Pts',(37.5483341381148,-29.1033264849348,4.26939975149549E-16));
#11246=CARTESIAN_POINT('Ctrl Pts',(37.5390498923763,-29.122691389158,1.61863618687202E-15));
#11247=CARTESIAN_POINT('Ctrl Pts',(37.5299909937341,-29.142178472125,1.60982338570648E-15));
#11248=CARTESIAN_POINT('Ctrl Pts',(37.5213410583467,-29.1607858122899,1.60140843774476E-15));
#11249=CARTESIAN_POINT('Ctrl Pts',(37.5128940924849,-29.179510547703,9.17086461423256E-17));
#11250=CARTESIAN_POINT('Ctrl Pts',(37.5046654270074,-29.1983159954623,1.66533453693773E-16));
#11251=CARTESIAN_POINT('Ctrl Pts',(37.4681044896221,-29.2818708318945,4.98988954677069E-16));
#11252=CARTESIAN_POINT('Ctrl Pts',(37.4358037760726,-29.3671091286622,3.22759138281679E-15));
#11253=CARTESIAN_POINT('Ctrl Pts',(37.4077875615482,-29.4536320411872,2.91433543964104E-15));
#11254=CARTESIAN_POINT('Ctrl Pts',(37.3793090722073,-29.5415826042421,2.59591069203894E-15));
#11255=CARTESIAN_POINT('Ctrl Pts',(37.3552571471219,-29.6308612814779,2.04735700495589E-15));
#11256=CARTESIAN_POINT('Ctrl Pts',(37.3356963907766,-29.7210862860857,1.55431223447522E-15));
#11257=CARTESIAN_POINT('Ctrl Pts',(37.3164739269567,-29.809750898849,1.06979440219971E-15));
#11258=CARTESIAN_POINT('Ctrl Pts',(37.3015883718447,-29.8993302989097,-4.96142364632893E-16));
#11259=CARTESIAN_POINT('Ctrl Pts',(37.2911437360475,-29.9894850121972,1.38777878078145E-16));
#11260=CARTESIAN_POINT('Ctrl Pts',(37.2870135672285,-30.0251352917219,3.89847215477509E-16));
#11261=CARTESIAN_POINT('Ctrl Pts',(37.2835783142426,-30.0608757129787,-2.36101949319689E-15));
#11262=CARTESIAN_POINT('Ctrl Pts',(37.2808464374724,-30.0966858197535,-2.74780198594726E-15));
#11263=CARTESIAN_POINT('Ctrl Pts',(37.2792295134997,-30.1178808534167,-2.97672808230688E-15));
#11264=CARTESIAN_POINT('Ctrl Pts',(37.2778590143499,-30.139100302959,-1.71621991249039E-15));
#11265=CARTESIAN_POINT('Ctrl Pts',(37.2767368966041,-30.1603399498113,-1.85962356624714E-15));
#11266=CARTESIAN_POINT('Ctrl Pts',(37.275989979541,-30.1744777305437,-1.95507757389332E-15));
#11267=CARTESIAN_POINT('Ctrl Pts',(37.2753531910632,-30.1886244564323,2.6775874477929E-15));
#11268=CARTESIAN_POINT('Ctrl Pts',(37.2748274592582,-30.2027643272738,2.60902410786912E-15));
#11269=CARTESIAN_POINT('Ctrl Pts',(37.271288634922,-30.2979431210418,2.147508153176E-15));
#11270=CARTESIAN_POINT('Ctrl Pts',(37.2727685565052,-30.3929728938572,1.24544634177833E-15));
#11271=CARTESIAN_POINT('Ctrl Pts',(37.2793258761199,-30.4874549271961,1.83186799063151E-15));
#11272=CARTESIAN_POINT('Ctrl Pts',(37.2858607014982,-30.5816128492639,2.41627797801546E-15));
#11273=CARTESIAN_POINT('Ctrl Pts',(37.2974377903602,-30.6752277367775,4.55832449058614E-16));
#11274=CARTESIAN_POINT('Ctrl Pts',(37.3141631908863,-30.7679228633085,2.77555756156289E-16));
#11275=CARTESIAN_POINT('Ctrl Pts',(37.3161000547763,-30.7786573053969,2.56910648831923E-16));
#11276=CARTESIAN_POINT('Ctrl Pts',(37.3181060167709,-30.7893794234663,4.5835681127338E-16));
#11277=CARTESIAN_POINT('Ctrl Pts',(37.3201812867948,-30.8000886389312,4.16333634234434E-16));
#11278=CARTESIAN_POINT('Ctrl Pts',(37.3377261922751,-30.8906273018195,6.31236541414227E-17));
#11279=CARTESIAN_POINT('Ctrl Pts',(37.3602204912016,-30.9802440608068,2.25684169593055E-15));
#11280=CARTESIAN_POINT('Ctrl Pts',(37.387388888656,-31.0687009861654,3.05311331771918E-15));
#11281=CARTESIAN_POINT('Ctrl Pts',(37.3981371536463,-31.1036960010747,3.36813147105597E-15));
#11282=CARTESIAN_POINT('Ctrl Pts',(37.4096175528861,-31.1385094369092,4.01162441398018E-15));
#11283=CARTESIAN_POINT('Ctrl Pts',(37.4218152344547,-31.1731262189978,3.88578058618805E-15));
#11284=CARTESIAN_POINT('Ctrl Pts',(37.427769072972,-31.1900230964399,3.82435466480679E-15));
#11285=CARTESIAN_POINT('Ctrl Pts',(37.4338938246471,-31.2068731161624,3.27596104949439E-15));
#11286=CARTESIAN_POINT('Ctrl Pts',(37.4401878632928,-31.2236744969284,3.44169137633799E-15));
#11287=CARTESIAN_POINT('Ctrl Pts',(37.445432955005,-31.2376758064166,3.57980154894933E-15));
#11288=CARTESIAN_POINT('Ctrl Pts',(37.4507927155412,-31.251635532049,4.17563321267137E-15));
#11289=CARTESIAN_POINT('Ctrl Pts',(37.4562639276339,-31.2655480863479,4.08006961549745E-15));
#11290=CARTESIAN_POINT('Ctrl Pts',(37.4904885203169,-31.3525766087289,3.48228156904737E-15));
#11291=CARTESIAN_POINT('Ctrl Pts',(37.5290915581906,-31.4378170268534,4.25521230771052E-15));
#11292=CARTESIAN_POINT('Ctrl Pts',(37.5717405530417,-31.5210374660102,3.89965837399586E-15));
#11293=CARTESIAN_POINT('Ctrl Pts',(37.6159697990177,-31.607341429012,3.53093028446207E-15));
#11294=CARTESIAN_POINT('Ctrl Pts',(37.6645505115892,-31.691473675336,8.20810124271393E-16));
#11295=CARTESIAN_POINT('Ctrl Pts',(37.7171678191012,-31.7731720613104,1.9151347174784E-15));
#11296=CARTESIAN_POINT('Ctrl Pts',(37.7703627831117,-31.8557673689594,3.0214732989067E-15));
#11297=CARTESIAN_POINT('Ctrl Pts',(37.8276838779193,-31.9358759006778,2.22421601072444E-15));
#11298=CARTESIAN_POINT('Ctrl Pts',(37.8888573645074,-32.0132114269328,3.02535774210355E-15));
#11299=CARTESIAN_POINT('Ctrl Pts',(37.9126742306003,-32.0433207108035,3.33726877418507E-15));
#11300=CARTESIAN_POINT('Ctrl Pts',(37.9370755579706,-32.07300943183,1.70170386855551E-15));
#11301=CARTESIAN_POINT('Ctrl Pts',(37.9620470578005,-32.1022596583239,1.67921232474555E-15));
#11302=CARTESIAN_POINT('Ctrl Pts',(37.9820283447379,-32.1256646268897,1.66121540851732E-15));
#11303=CARTESIAN_POINT('Ctrl Pts',(38.0023747117564,-32.1487888334358,3.62130422901362E-15));
#11304=CARTESIAN_POINT('Ctrl Pts',(38.0230792744415,-32.171622749665,3.87190279838023E-15));
#11305=CARTESIAN_POINT('Ctrl Pts',(38.0346329406524,-32.1843646486566,4.01174309674448E-15));
#11306=CARTESIAN_POINT('Ctrl Pts',(38.0462930844947,-32.1970105005967,2.59157039562667E-15));
#11307=CARTESIAN_POINT('Ctrl Pts',(38.0580534283639,-32.2095538559179,2.42861286636753E-15));
#11308=CARTESIAN_POINT('Ctrl Pts',(38.1271088212578,-32.2832070024204,1.4717449096841E-15));
#11309=CARTESIAN_POINT('Ctrl Pts',(38.199664805144,-32.3533827208338,3.45538810407262E-15));
#11310=CARTESIAN_POINT('Ctrl Pts',(38.275409437109,-32.4197921562816,3.53883589099269E-15));
#11311=CARTESIAN_POINT('Ctrl Pts',(38.3396605957844,-32.4761246390439,3.60962132963588E-15));
#11312=CARTESIAN_POINT('Ctrl Pts',(38.4062071932438,-32.529747132498,5.98119156967079E-15));
#11313=CARTESIAN_POINT('Ctrl Pts',(38.4748836902505,-32.5804684054025,6.17561557447743E-15));
#11314=CARTESIAN_POINT('Ctrl Pts',(38.4975706616452,-32.5972239494044,6.23984266857442E-15));
#11315=CARTESIAN_POINT('Ctrl Pts',(38.5204902321351,-32.6136627516457,2.07827934435607E-15));
#11316=CARTESIAN_POINT('Ctrl Pts',(38.5436369048366,-32.6297774777457,1.62370117351429E-15));
#11317=CARTESIAN_POINT('Ctrl Pts',(38.5602345029377,-32.6413327345538,1.29774046708829E-15));
#11318=CARTESIAN_POINT('Ctrl Pts',(38.5769498432321,-32.6527218838852,5.07588258890606E-15));
#11319=CARTESIAN_POINT('Ctrl Pts',(38.5937663318716,-32.6639327287669,4.86416462663897E-15));
#11320=CARTESIAN_POINT('Ctrl Pts',(38.6801203281873,-32.7215013019905,3.77697618169038E-15));
#11321=CARTESIAN_POINT('Ctrl Pts',(38.7692237115985,-32.7744316059974,-2.13679161323202E-15));
#11322=CARTESIAN_POINT('Ctrl Pts',(38.8607679331194,-32.8224021724615,-2.24126273096203E-15));
#11323=CARTESIAN_POINT('Ctrl Pts',(38.9523121546403,-32.8703727389257,-2.34573384869205E-15));
#11324=CARTESIAN_POINT('Ctrl Pts',(39.0462978596107,-32.9133844785481,-2.61326211847443E-15));
#11325=CARTESIAN_POINT('Ctrl Pts',(39.1424545426358,-32.9510751762973,-3.60171961699685E-15));
#11326=CARTESIAN_POINT('Ctrl Pts',(39.1630225201047,-32.9591372412282,-3.77498740676788E-15));
#11327=CARTESIAN_POINT('Ctrl Pts',(39.1836899454549,-32.9669556727912,-2.23961353901364E-15));
#11328=CARTESIAN_POINT('Ctrl Pts',(39.2044529144508,-32.9745316477842,-2.27595720048157E-15));
#11329=CARTESIAN_POINT('Ctrl Pts',(37.4857778982365,-29.998587099551,9.11258330249199));
#11330=CARTESIAN_POINT('Ctrl Pts',(37.4840985574538,-29.6714493670241,9.09196520028265));
#11331=CARTESIAN_POINT('Ctrl Pts',(37.543355536012,-29.3448947567928,9.07134709807331));
#11332=CARTESIAN_POINT('Ctrl Pts',(37.66637530026,-29.044450672095,9.05072899586396));
#11333=CARTESIAN_POINT('Ctrl Pts',(37.9821764108085,-28.2731878088856,8.99780075612207));
#11334=CARTESIAN_POINT('Ctrl Pts',(38.7181666456359,-27.6739901830981,8.94487251638018));
#11335=CARTESIAN_POINT('Ctrl Pts',(39.5374366241675,-27.5211158178176,8.89194427663828));
#11336=CARTESIAN_POINT('Ctrl Pts',(40.3567066026992,-27.368241452537,8.83901603689639));
#11337=CARTESIAN_POINT('Ctrl Pts',(41.2592563249352,-27.6616903477634,8.78608779715449));
#11338=CARTESIAN_POINT('Ctrl Pts',(41.8319590891433,-28.2671485834999,8.7331595574126));
#11339=CARTESIAN_POINT('Ctrl Pts',(42.4046618533514,-28.8726068192364,8.68023131767071));
#11340=CARTESIAN_POINT('Ctrl Pts',(42.6475176595316,-29.7900743954829,8.62730307792881));
#11341=CARTESIAN_POINT('Ctrl Pts',(42.4493572717447,-30.5995831543275,8.57437483818692));
#11342=CARTESIAN_POINT('Ctrl Pts',(42.2511968839578,-31.409091913172,8.52144659844502));
#11343=CARTESIAN_POINT('Ctrl Pts',(41.6120203022038,-32.1106418546146,8.46851835870312));
#11344=CARTESIAN_POINT('Ctrl Pts',(40.8244073292669,-32.3831067682726,8.41559011896123));
#11345=CARTESIAN_POINT('Ctrl Pts',(40.0367943563299,-32.6555716819306,8.36266187921934));
#11346=CARTESIAN_POINT('Ctrl Pts',(39.10074499221,-32.4989515678041,8.30973363947745));
#11347=CARTESIAN_POINT('Ctrl Pts',(38.444727099256,-31.9849367469148,8.25680539973555));
#11348=CARTESIAN_POINT('Ctrl Pts',(37.8488745713017,-31.5180637641465,8.20873136732103));
#11349=CARTESIAN_POINT('Ctrl Pts',(37.4840438865339,-30.7563454071862,8.16065733490651));
#11350=CARTESIAN_POINT('Ctrl Pts',(37.4791974871636,-29.9986726512116,8.11258330249198));
#11351=CARTESIAN_POINT('Origin',(-40.,30.,12.2084234471774));
#11352=CARTESIAN_POINT('Ctrl Pts',(-43.0762854577871,30.0022177574501,9.70842344717746));
#11353=CARTESIAN_POINT('Ctrl Pts',(-43.0774828058572,30.147004819194,9.70090492237387));
#11354=CARTESIAN_POINT('Ctrl Pts',(-43.0023604322999,31.3098385439038,9.64045815782839));
#11355=CARTESIAN_POINT('Ctrl Pts',(-41.5191022135468,33.3003381593159,9.52708315354102));
#11356=CARTESIAN_POINT('Ctrl Pts',(-38.0509703519274,33.065699819527,9.36829843431533));
#11357=CARTESIAN_POINT('Ctrl Pts',(-36.3671810948824,30.024955201687,9.20951371508965));
#11358=CARTESIAN_POINT('Ctrl Pts',(-38.0091584240807,26.9611184995217,9.05072899586397));
#11359=CARTESIAN_POINT('Ctrl Pts',(-41.4737278989921,26.6794508066113,8.89194427663828));
#11360=CARTESIAN_POINT('Ctrl Pts',(-42.993836649437,28.661463151569,8.77784242707611));
#11361=CARTESIAN_POINT('Ctrl Pts',(-43.0772715769482,29.8387134364101,8.71666881725584));
#11362=CARTESIAN_POINT('Ctrl Pts',(-43.0759023900792,29.9975851856081,8.70842344717746));
#11363=CARTESIAN_POINT('Ctrl Pts',(-43.070401160077,29.9965365385191,9.79157655282254));
#11364=CARTESIAN_POINT('Ctrl Pts',(-43.0650787483756,30.7003379664639,9.75519455573124));
#11365=CARTESIAN_POINT('Ctrl Pts',(-42.4772111316602,32.4385313995888,9.66588431889804));
#11366=CARTESIAN_POINT('Ctrl Pts',(-39.5908856649077,33.609025071703,9.52364584232295));
#11367=CARTESIAN_POINT('Ctrl Pts',(-36.7458102038522,31.6147488878258,9.36486112309727));
#11368=CARTESIAN_POINT('Ctrl Pts',(-36.8786563309339,28.140667484321,9.20607640387158));
#11369=CARTESIAN_POINT('Ctrl Pts',(-39.869659490377,26.3695393883571,9.0472916846459));
#11370=CARTESIAN_POINT('Ctrl Pts',(-42.5758435358444,27.7201136457931,8.90912506762955));
#11371=CARTESIAN_POINT('Ctrl Pts',(-43.0662857206963,29.3758543810734,8.8238866903551));
#11372=CARTESIAN_POINT('Ctrl Pts',(-43.0694985803644,30.001724961275,8.79157655282254));
#11373=CARTESIAN_POINT('Ctrl Pts',(-38.0865340033349,31.635987203375,10.));
#11374=CARTESIAN_POINT('Ctrl Pts',(-37.5424734719262,30.999648896553,9.94707176025811));
#11375=CARTESIAN_POINT('Ctrl Pts',(-37.1490014826279,29.1520157886412,9.84121528077432));
#11376=CARTESIAN_POINT('Ctrl Pts',(-39.1694212746662,27.1407133917689,9.68243056154863));
#11377=CARTESIAN_POINT('Ctrl Pts',(-41.9506454231488,27.7536503742996,9.52364584232295));
#11378=CARTESIAN_POINT('Ctrl Pts',(-42.9458435401314,30.41986209395,9.36486112309726));
#11379=CARTESIAN_POINT('Ctrl Pts',(-41.2442947202227,32.7033028521483,9.20607640387159));
#11380=CARTESIAN_POINT('Ctrl Pts',(-38.4035522567032,32.5111108819453,9.0472916846459));
#11381=CARTESIAN_POINT('Ctrl Pts',(-37.0243625854454,30.0204407744419,8.88850696542021));
#11382=CARTESIAN_POINT('Ctrl Pts',(-38.3693041589794,27.5108559695935,8.72972224619454));
#11383=CARTESIAN_POINT('Ctrl Pts',(-41.2071286760087,27.2801423151599,8.57093752696885));
#11384=CARTESIAN_POINT('Ctrl Pts',(-42.9398429054373,29.5393629084276,8.41215280774317));
#11385=CARTESIAN_POINT('Ctrl Pts',(-41.9811814845473,32.2203144553808,8.25336808851748));
#11386=CARTESIAN_POINT('Ctrl Pts',(-39.2087801576347,32.8685921237222,8.09458336929179));
#11387=CARTESIAN_POINT('Ctrl Pts',(-37.1607280190766,30.8907274356912,7.93579865006612));
#11388=CARTESIAN_POINT('Ctrl Pts',(-37.7119822297206,28.0974133164057,7.77701393084042));
#11389=CARTESIAN_POINT('Ctrl Pts',(-40.3578790364915,27.0458874682206,7.61822921161475));
#11390=CARTESIAN_POINT('Ctrl Pts',(-42.6761434353152,28.6988020463829,7.45944449238906));
#11391=CARTESIAN_POINT('Ctrl Pts',(-42.5444427578219,31.5429422554505,7.30065977316338));
#11392=CARTESIAN_POINT('Ctrl Pts',(-40.0833467521405,32.9745441179435,7.1418750539377));
#11393=CARTESIAN_POINT('Ctrl Pts',(-37.5459481794697,31.683000077592,6.98309033471201));
#11394=CARTESIAN_POINT('Ctrl Pts',(-37.2551935056625,28.8506972178761,6.82430561548633));
#11395=CARTESIAN_POINT('Ctrl Pts',(-39.4772638374019,27.0705620947472,6.66552089626065));
#11396=CARTESIAN_POINT('Ctrl Pts',(-42.1778904898475,27.9722789693785,6.50673617703496));
#11397=CARTESIAN_POINT('Ctrl Pts',(-42.8846943763049,30.7303409575371,6.34795145780928));
#11398=CARTESIAN_POINT('Ctrl Pts',(-40.9506082138133,32.8197878605566,6.18916673858359));
#11399=CARTESIAN_POINT('Ctrl Pts',(-38.1462559349721,32.3277655594152,6.03038201935791));
#11400=CARTESIAN_POINT('Ctrl Pts',(-37.0389757252595,29.704712340631,5.87159730013223));
#11401=CARTESIAN_POINT('Ctrl Pts',(-38.6424643253917,27.3519900964832,5.71281258090655));
#11402=CARTESIAN_POINT('Ctrl Pts',(-41.4887544102281,27.4234771758386,5.55402786168086));
#11403=CARTESIAN_POINT('Ctrl Pts',(-42.9721144255193,29.8537283387532,5.39524314245518));
#11404=CARTESIAN_POINT('Ctrl Pts',(-41.734552781155,32.4178887912006,5.23645842322949));
#11405=CARTESIAN_POINT('Ctrl Pts',(-38.9090367190449,32.768511996884,5.07767370400381));
#11406=CARTESIAN_POINT('Ctrl Pts',(-37.0822795188237,30.5846082029712,4.91888898477813));
#11407=CARTESIAN_POINT('Ctrl Pts',(-37.9266472207506,27.8655052564986,4.76010426555244));
#11408=CARTESIAN_POINT('Ctrl Pts',(-40.6691351419837,27.1004969875778,4.60131954632676));
#11409=CARTESIAN_POINT('Ctrl Pts',(-42.7990408942909,28.9899358291112,4.44253482710108));
#11410=CARTESIAN_POINT('Ctrl Pts',(-42.3664709457677,31.8040717336351,4.28375010787539));
#11411=CARTESIAN_POINT('Ctrl Pts',(-39.7674359385366,32.9666097678519,4.12496538864971));
#11412=CARTESIAN_POINT('Ctrl Pts',(-37.3813094878688,31.4132655655012,3.96618066942403));
#11413=CARTESIAN_POINT('Ctrl Pts',(-37.3925509422966,28.5661000840857,3.80739595019834));
#11414=CARTESIAN_POINT('Ctrl Pts',(-39.7908689363652,27.0316462885214,3.64861123097266));
#11415=CARTESIAN_POINT('Ctrl Pts',(-42.3806429640183,28.2146712816453,3.48982651174698));
#11416=CARTESIAN_POINT('Ctrl Pts',(-42.7909776853917,31.0321352230143,3.33104179252129));
#11417=CARTESIAN_POINT('Ctrl Pts',(-40.6462184384815,32.9046964202063,3.17225707329561));
#11418=CARTESIAN_POINT('Ctrl Pts',(-37.9098568901123,32.1180560230099,3.01347235406992));
#11419=CARTESIAN_POINT('Ctrl Pts',(-37.0869868234582,29.3923703351144,2.85468763484424));
#11420=CARTESIAN_POINT('Ctrl Pts',(-38.9309322151455,27.2229595482945,2.69590291561856));
#11421=CARTESIAN_POINT('Ctrl Pts',(-41.7535914721387,27.5958834596619,2.53711819639287));
#11422=CARTESIAN_POINT('Ctrl Pts',(-42.9708667673923,30.1697362715842,2.37833347716719));
#11423=CARTESIAN_POINT('Ctrl Pts',(-41.4683624873955,32.5881984866867,2.2195487579415));
#11424=CARTESIAN_POINT('Ctrl Pts',(-38.6215968579575,32.6372074308222,2.06076403871582));
#11425=CARTESIAN_POINT('Ctrl Pts',(-37.0367360325092,30.27189715827,1.90197931949014));
#11426=CARTESIAN_POINT('Ctrl Pts',(-38.1646954219365,27.6576682873493,1.74319460026445));
#11427=CARTESIAN_POINT('Ctrl Pts',(-40.9728438312614,27.1878078850814,1.58440988103877));
#11428=CARTESIAN_POINT('Ctrl Pts',(-42.8903737846055,29.2924579583155,1.42562516181309));
#11429=CARTESIAN_POINT('Ctrl Pts',(-42.1618062952702,32.0448609685045,1.2668404425874));
#11430=CARTESIAN_POINT('Ctrl Pts',(-39.4541568081119,32.9252078004982,1.10805572336172));
#11431=CARTESIAN_POINT('Ctrl Pts',(-37.24618588728,31.1276146339126,0.949271004136038));
#11432=CARTESIAN_POINT('Ctrl Pts',(-37.5593499150186,28.2976301780055,0.790486284910354));
#11433=CARTESIAN_POINT('Ctrl Pts',(-40.1067617368674,27.0262943672847,0.63170156568467));
#11434=CARTESIAN_POINT('Ctrl Pts',(-42.556688642221,28.4770230310523,0.472916846458986));
#11435=CARTESIAN_POINT('Ctrl Pts',(-42.665502715148,31.3226388835994,0.314132127233303));
#11436=CARTESIAN_POINT('Ctrl Pts',(-40.3351050257151,32.9561476332342,0.155347408007618));
#11437=CARTESIAN_POINT('Ctrl Pts',(-37.695899841043,31.8858693975142,-0.00343731121806418));
#11438=CARTESIAN_POINT('Ctrl Pts',(-37.1701531156465,29.0839015446546,-0.162222030443749));
#11439=CARTESIAN_POINT('Ctrl Pts',(-38.5409902294193,27.7841423687619,-0.268078509927538));
#11440=CARTESIAN_POINT('Ctrl Pts',(-39.3498000020249,27.5679131979649,-0.321006749669432));
#11441=CARTESIAN_POINT('Ctrl Pts',(-37.9456684496579,31.7564253212269,10.1070022498898));
#11442=CARTESIAN_POINT('Ctrl Pts',(-37.3615552660859,31.0732410562992,10.0540740101479));
#11443=CARTESIAN_POINT('Ctrl Pts',(-36.939116653014,29.0895888807941,9.94821753066413));
#11444=CARTESIAN_POINT('Ctrl Pts',(-39.108275724016,26.9302184094218,9.78943281143844));
#11445=CARTESIAN_POINT('Ctrl Pts',(-42.0942480521154,27.5882785911961,9.63064809221277));
#11446=CARTESIAN_POINT('Ctrl Pts',(-43.1627106713215,30.45077150464,9.47186337298707));
#11447=CARTESIAN_POINT('Ctrl Pts',(-41.3358972179974,32.9023146212042,9.3130786537614));
#11448=CARTESIAN_POINT('Ctrl Pts',(-38.2860249551112,32.6959738611392,9.15429393453571));
#11449=CARTESIAN_POINT('Ctrl Pts',(-36.8053020885911,30.0219455835236,8.99550921531003));
#11450=CARTESIAN_POINT('Ctrl Pts',(-38.2492555806798,27.3276101462363,8.83672449608435));
#11451=CARTESIAN_POINT('Ctrl Pts',(-41.2959950836698,27.0799118123104,8.67793977685866));
#11452=CARTESIAN_POINT('Ctrl Pts',(-43.1562682818588,29.5054517236657,8.51915505763298));
#11453=CARTESIAN_POINT('Ctrl Pts',(-42.1270321175044,32.3837695811262,8.3603703384073));
#11454=CARTESIAN_POINT('Ctrl Pts',(-39.1505321295175,33.0797721595765,8.2015856191816));
#11455=CARTESIAN_POINT('Ctrl Pts',(-36.9517064737084,30.9563010145385,8.04280089995593));
#11456=CARTESIAN_POINT('Ctrl Pts',(-37.5435429208461,27.9573486760775,7.88401618073024));
#11457=CARTESIAN_POINT('Ctrl Pts',(-40.3842253780061,26.8284115903431,7.72523146150456));
#11458=CARTESIAN_POINT('Ctrl Pts',(-42.8731557822249,28.6030104459577,7.56644674227887));
#11459=CARTESIAN_POINT('Ctrl Pts',(-42.7317595632967,31.6565305896485,7.40766202305319));
#11460=CARTESIAN_POINT('Ctrl Pts',(-40.0894825739465,33.19352412848,7.2488773038275));
#11461=CARTESIAN_POINT('Ctrl Pts',(-37.3652857746746,31.8068991895604,7.09009258460182));
#11462=CARTESIAN_POINT('Ctrl Pts',(-37.0531263211737,28.7660878372921,6.93130786537614));
#11463=CARTESIAN_POINT('Ctrl Pts',(-39.438781042777,26.8549027137051,6.77252314615046));
#11464=CARTESIAN_POINT('Ctrl Pts',(-42.3382224477893,27.8230021877797,6.61373842692476));
#11465=CARTESIAN_POINT('Ctrl Pts',(-43.0970598279071,30.7841072034677,6.45495370769909));
#11466=CARTESIAN_POINT('Ctrl Pts',(-41.0205900962205,33.0273750238097,6.2961689884734));
#11467=CARTESIAN_POINT('Ctrl Pts',(-38.0097869908933,32.4991310213199,6.13738426924772));
#11468=CARTESIAN_POINT('Ctrl Pts',(-36.8209910186385,29.6829738515732,5.97859955002204));
#11469=CARTESIAN_POINT('Ctrl Pts',(-38.5425252542124,27.1570488841224,5.81981483079635));
#11470=CARTESIAN_POINT('Ctrl Pts',(-41.5983535432419,27.2337986998063,5.66103011157068));
#11471=CARTESIAN_POINT('Ctrl Pts',(-43.1909155669411,29.8429601105304,5.50224539234498));
#11472=CARTESIAN_POINT('Ctrl Pts',(-41.8622471004298,32.5958889458391,5.34346067311931));
#11473=CARTESIAN_POINT('Ctrl Pts',(-38.8287221762828,32.9723243332319,5.18467595389361));
#11474=CARTESIAN_POINT('Ctrl Pts',(-36.8674827511926,30.6276458939148,5.02589123466794));
#11475=CARTESIAN_POINT('Ctrl Pts',(-37.7740111207489,27.7083680069273,4.86710651544225));
#11476=CARTESIAN_POINT('Ctrl Pts',(-40.7183955377391,26.8870413536941,4.70832179621658));
#11477=CARTESIAN_POINT('Ctrl Pts',(-43.0051007072304,28.915576917623,4.54953707699088));
#11478=CARTESIAN_POINT('Ctrl Pts',(-42.5406858210866,31.9368838996598,4.3907523577652));
#11479=CARTESIAN_POINT('Ctrl Pts',(-39.7503150357662,33.1850056673455,4.23196763853952));
#11480=CARTESIAN_POINT('Ctrl Pts',(-37.1885267106766,31.5173073601942,4.07318291931384));
#11481=CARTESIAN_POINT('Ctrl Pts',(-37.2005957385781,28.4605392296337,3.91439820008815));
#11482=CARTESIAN_POINT('Ctrl Pts',(-39.7754731241996,26.8131220033732,3.75561348086247));
#11483=CARTESIAN_POINT('Ctrl Pts',(-42.5559011550801,28.0832389390561,3.59682876163678));
#11484=CARTESIAN_POINT('Ctrl Pts',(-42.9964439009598,31.1081189613785,3.4380440424111));
#11485=CARTESIAN_POINT('Ctrl Pts',(-40.6937917521916,33.1185343824222,3.27925932318542));
#11486=CARTESIAN_POINT('Ctrl Pts',(-37.7559847194274,32.2739830867363,3.12047460395973));
#11487=CARTESIAN_POINT('Ctrl Pts',(-36.8725365982139,29.3476378500199,2.96168988473406));
#11488=CARTESIAN_POINT('Ctrl Pts',(-38.8522295751747,27.0185193640974,2.80290516550837));
#11489=CARTESIAN_POINT('Ctrl Pts',(-41.8826873819049,27.4188971906877,2.64412044628269));
#11490=CARTESIAN_POINT('Ctrl Pts',(-43.1895760587091,30.1822319176617,2.485335727057));
#11491=CARTESIAN_POINT('Ctrl Pts',(-41.5764604076857,32.7787365017279,2.32655100783132));
#11492=CARTESIAN_POINT('Ctrl Pts',(-38.5201215654086,32.8313533866695,2.16776628860563));
#11493=CARTESIAN_POINT('Ctrl Pts',(-36.8185864441709,30.2919136852476,2.00898156937995));
#11494=CARTESIAN_POINT('Ctrl Pts',(-38.0295839561433,27.4852304942697,1.85019685015426));
#11495=CARTESIAN_POINT('Ctrl Pts',(-41.0444626555158,26.9807799054859,1.69141213092858));
#11496=CARTESIAN_POINT('Ctrl Pts',(-43.1031573429294,29.2403701231382,1.5326274117029));
#11497=CARTESIAN_POINT('Ctrl Pts',(-42.3209541668584,32.1953995581752,1.37384269247722));
#11498=CARTESIAN_POINT('Ctrl Pts',(-39.4139729200365,33.1405557696577,1.21505797325153));
#11499=CARTESIAN_POINT('Ctrl Pts',(-37.0434555798755,31.2106273762437,1.05627325402585));
#11500=CARTESIAN_POINT('Ctrl Pts',(-37.3796741192888,28.1723051040527,0.897488534800164));
#11501=CARTESIAN_POINT('Ctrl Pts',(-40.1146213231896,26.8073760843598,0.738703815574481));
#11502=CARTESIAN_POINT('Ctrl Pts',(-42.7449069653027,28.3649045014615,0.579919096348796));
#11503=CARTESIAN_POINT('Ctrl Pts',(-42.8617317134429,31.4200089225642,0.421134377123114));
#11504=CARTESIAN_POINT('Ctrl Pts',(-40.3597747899385,33.1737733312253,0.262349657897429));
#11505=CARTESIAN_POINT('Ctrl Pts',(-37.5262765787616,32.024703344554,0.103564938671747));
#11506=CARTESIAN_POINT('Ctrl Pts',(-36.9618254271062,29.0164602018976,-0.0552197805539385));
#11507=CARTESIAN_POINT('Ctrl Pts',(-38.4335808375036,27.6210153455288,-0.161076260037727));
#11508=CARTESIAN_POINT('Ctrl Pts',(-39.301933573839,27.3888678140614,-0.214004499779622));
#11509=CARTESIAN_POINT('Ctrl Pts',(-37.8048028959809,31.8768634390788,10.2140044997796));
#11510=CARTESIAN_POINT('Ctrl Pts',(-37.1806370602456,31.1468332160454,10.1610762600377));
#11511=CARTESIAN_POINT('Ctrl Pts',(-36.7292318234001,29.027161972947,10.0552197805539));
#11512=CARTESIAN_POINT('Ctrl Pts',(-39.0471301733659,26.7197234270748,9.89643506132826));
#11513=CARTESIAN_POINT('Ctrl Pts',(-42.2378506810821,27.4229068080925,9.73765034210257));
#11514=CARTESIAN_POINT('Ctrl Pts',(-43.3795778025116,30.4816809153299,9.57886562287688));
#11515=CARTESIAN_POINT('Ctrl Pts',(-41.4274997157721,33.10132639026,9.42008090365121));
#11516=CARTESIAN_POINT('Ctrl Pts',(-38.1684976535193,32.8808368403331,9.26129618442551));
#11517=CARTESIAN_POINT('Ctrl Pts',(-36.5862415917368,30.0234503926053,9.10251146519984));
#11518=CARTESIAN_POINT('Ctrl Pts',(-38.1292070023802,27.144364322879,8.94372674597416));
#11519=CARTESIAN_POINT('Ctrl Pts',(-41.384861491331,26.8796813094609,8.78494202674847));
#11520=CARTESIAN_POINT('Ctrl Pts',(-43.3726936582803,29.4715405389038,8.62615730752279));
#11521=CARTESIAN_POINT('Ctrl Pts',(-42.2728827504615,32.5472247068716,8.4673725882971));
#11522=CARTESIAN_POINT('Ctrl Pts',(-39.0922841014003,33.2909521954307,8.30858786907142));
#11523=CARTESIAN_POINT('Ctrl Pts',(-36.7426849283402,31.0218745933858,8.14980314984573));
#11524=CARTESIAN_POINT('Ctrl Pts',(-37.3751036119715,27.8172840357493,7.99101843062005));
#11525=CARTESIAN_POINT('Ctrl Pts',(-40.4105717195208,26.6109357124657,7.83223371139437));
#11526=CARTESIAN_POINT('Ctrl Pts',(-43.0701681291345,28.5072188455325,7.67344899216868));
#11527=CARTESIAN_POINT('Ctrl Pts',(-42.9190763687717,31.7701189238465,7.51466427294301));
#11528=CARTESIAN_POINT('Ctrl Pts',(-40.0956183957525,33.4125041390164,7.35587955371731));
#11529=CARTESIAN_POINT('Ctrl Pts',(-37.1846233698796,31.9307983015287,7.19709483449163));
#11530=CARTESIAN_POINT('Ctrl Pts',(-36.8510591366849,28.6814784567081,7.03831011526595));
#11531=CARTESIAN_POINT('Ctrl Pts',(-39.4002982481521,26.639243332663,6.87952539604027));
#11532=CARTESIAN_POINT('Ctrl Pts',(-42.4985544057311,27.6737254061808,6.72074067681458));
#11533=CARTESIAN_POINT('Ctrl Pts',(-43.3094252795093,30.8378734493983,6.56195595758889));
#11534=CARTESIAN_POINT('Ctrl Pts',(-41.0905719786276,33.2349621870629,6.40317123836322));
#11535=CARTESIAN_POINT('Ctrl Pts',(-37.8733180468145,32.6704964832245,6.24438651913753));
#11536=CARTESIAN_POINT('Ctrl Pts',(-36.6030063120174,29.6612353625154,6.08560179991185));
#11537=CARTESIAN_POINT('Ctrl Pts',(-38.442586183033,26.9621076717615,5.92681708068616));
#11538=CARTESIAN_POINT('Ctrl Pts',(-41.7079526762557,27.044120223774,5.76803236146049));
#11539=CARTESIAN_POINT('Ctrl Pts',(-43.409716708363,29.8321918823075,5.60924764223479));
#11540=CARTESIAN_POINT('Ctrl Pts',(-41.9899414197044,32.7738891004776,5.45046292300912));
#11541=CARTESIAN_POINT('Ctrl Pts',(-38.7484076335206,33.1761366695798,5.29167820378343));
#11542=CARTESIAN_POINT('Ctrl Pts',(-36.6526859835615,30.6706835848585,5.13289348455775));
#11543=CARTESIAN_POINT('Ctrl Pts',(-37.6213750207472,27.5512307573561,4.97410876533206));
#11544=CARTESIAN_POINT('Ctrl Pts',(-40.7676559334946,26.6735857198104,4.81532404610638));
#11545=CARTESIAN_POINT('Ctrl Pts',(-43.2111605201699,28.8412180061349,4.6565393268807));
#11546=CARTESIAN_POINT('Ctrl Pts',(-42.7149006964056,32.0696960656844,4.49775460765501));
#11547=CARTESIAN_POINT('Ctrl Pts',(-39.7331941329958,33.4034015668391,4.33896988842933));
#11548=CARTESIAN_POINT('Ctrl Pts',(-36.9957439334843,31.6213491548871,4.18018516920365));
#11549=CARTESIAN_POINT('Ctrl Pts',(-37.0086405348597,28.3549783751818,4.02140044997796));
#11550=CARTESIAN_POINT('Ctrl Pts',(-39.760077312034,26.594597718225,3.86261573075228));
#11551=CARTESIAN_POINT('Ctrl Pts',(-42.7311593461418,27.9518065964668,3.7038310115266));
#11552=CARTESIAN_POINT('Ctrl Pts',(-43.2019101165279,31.1841026997428,3.54504629230091));
#11553=CARTESIAN_POINT('Ctrl Pts',(-40.7413650659017,33.3323723446379,3.38626157307523));
#11554=CARTESIAN_POINT('Ctrl Pts',(-37.6021125487425,32.4299101504626,3.22747685384954));
#11555=CARTESIAN_POINT('Ctrl Pts',(-36.6580863729697,29.3029053649254,3.06869213462386));
#11556=CARTESIAN_POINT('Ctrl Pts',(-38.773526935204,26.8140791799003,2.90990741539818));
#11557=CARTESIAN_POINT('Ctrl Pts',(-42.011783291671,27.2419109217134,2.75112269617249));
#11558=CARTESIAN_POINT('Ctrl Pts',(-43.4082853500259,30.1947275637393,2.59233797694681));
#11559=CARTESIAN_POINT('Ctrl Pts',(-41.6845583279759,32.9692745167689,2.43355325772113));
#11560=CARTESIAN_POINT('Ctrl Pts',(-38.4186462728598,33.0254993425169,2.27476853849544));
#11561=CARTESIAN_POINT('Ctrl Pts',(-36.6004368558326,30.3119302122251,2.11598381926976));
#11562=CARTESIAN_POINT('Ctrl Pts',(-37.8944724903502,27.3127927011901,1.95719910004407));
#11563=CARTESIAN_POINT('Ctrl Pts',(-41.1160814797701,26.7737519258905,1.79841438081839));
#11564=CARTESIAN_POINT('Ctrl Pts',(-43.3159409012533,29.1882822879609,1.63962966159271));
#11565=CARTESIAN_POINT('Ctrl Pts',(-42.4801020384466,32.345938147846,1.48084494236703));
#11566=CARTESIAN_POINT('Ctrl Pts',(-39.373789031961,33.3559037388171,1.32206022314134));
#11567=CARTESIAN_POINT('Ctrl Pts',(-36.840725272471,31.2936401185748,1.16327550391566));
#11568=CARTESIAN_POINT('Ctrl Pts',(-37.199998323559,28.0469800300999,1.00449078468998));
#11569=CARTESIAN_POINT('Ctrl Pts',(-40.1224809095117,26.588457801435,0.845706065464291));
#11570=CARTESIAN_POINT('Ctrl Pts',(-42.9331252883845,28.2527859718707,0.686921346238608));
#11571=CARTESIAN_POINT('Ctrl Pts',(-43.0579607117377,31.5173789615289,0.528136627012924));
#11572=CARTESIAN_POINT('Ctrl Pts',(-40.384444554162,33.3913990292165,0.36935190778724));
#11573=CARTESIAN_POINT('Ctrl Pts',(-37.3566533164802,32.1635372915938,0.210567188561557));
#11574=CARTESIAN_POINT('Ctrl Pts',(-36.7534977385659,28.9490188591406,0.0517824693358725));
#11575=CARTESIAN_POINT('Ctrl Pts',(-38.326171445588,27.4578883222956,-0.0540740101479163));
#11576=CARTESIAN_POINT('Ctrl Pts',(-39.254067145653,27.2098224301578,-0.107002249889811));
#11577=CARTESIAN_POINT('Ctrl Pts',(-37.6639373423039,31.9973015569307,10.3210067496694));
#11578=CARTESIAN_POINT('Ctrl Pts',(-36.9997188544053,31.2204253757917,10.2680785099275));
#11579=CARTESIAN_POINT('Ctrl Pts',(-36.5193469937862,28.9647350650998,10.1622220304437));
#11580=CARTESIAN_POINT('Ctrl Pts',(-38.9859846227157,26.5092284447277,10.0034373112181));
#11581=CARTESIAN_POINT('Ctrl Pts',(-42.3814533100487,27.2575350249889,9.84465259199239));
#11582=CARTESIAN_POINT('Ctrl Pts',(-43.5964449337017,30.51259032602,9.6858678727667));
#11583=CARTESIAN_POINT('Ctrl Pts',(-41.5191022135468,33.3003381593159,9.52708315354102));
#11584=CARTESIAN_POINT('Ctrl Pts',(-38.0509703519274,33.065699819527,9.36829843431533));
#11585=CARTESIAN_POINT('Ctrl Pts',(-36.3671810948824,30.024955201687,9.20951371508965));
#11586=CARTESIAN_POINT('Ctrl Pts',(-38.0091584240807,26.9611184995217,9.05072899586397));
#11587=CARTESIAN_POINT('Ctrl Pts',(-41.4737278989921,26.6794508066113,8.89194427663828));
#11588=CARTESIAN_POINT('Ctrl Pts',(-43.5891190347018,29.4376293541419,8.7331595574126));
#11589=CARTESIAN_POINT('Ctrl Pts',(-42.4187333834185,32.7106798326169,8.57437483818692));
#11590=CARTESIAN_POINT('Ctrl Pts',(-39.0340360732831,33.502132231285,8.41559011896122));
#11591=CARTESIAN_POINT('Ctrl Pts',(-36.533663382972,31.0874481722331,8.25680539973555));
#11592=CARTESIAN_POINT('Ctrl Pts',(-37.2066643030969,27.6772193954211,8.09802068050986));
#11593=CARTESIAN_POINT('Ctrl Pts',(-40.4369180610355,26.3934598345883,7.93923596128418));
#11594=CARTESIAN_POINT('Ctrl Pts',(-43.2671804760441,28.4114272451073,7.7804512420585));
#11595=CARTESIAN_POINT('Ctrl Pts',(-43.1063931742466,31.8837072580445,7.62166652283282));
#11596=CARTESIAN_POINT('Ctrl Pts',(-40.1017542175585,33.6314841495529,7.46288180360712));
#11597=CARTESIAN_POINT('Ctrl Pts',(-37.0039609650845,32.0546974134971,7.30409708438145));
#11598=CARTESIAN_POINT('Ctrl Pts',(-36.6489919521961,28.596869076124,7.14531236515576));
#11599=CARTESIAN_POINT('Ctrl Pts',(-39.3618154535272,26.4235839516209,6.98652764593008));
#11600=CARTESIAN_POINT('Ctrl Pts',(-42.6588863636729,27.5244486245819,6.82774292670439));
#11601=CARTESIAN_POINT('Ctrl Pts',(-43.5217907311115,30.8916396953289,6.66895820747871));
#11602=CARTESIAN_POINT('Ctrl Pts',(-41.1605538610348,33.4425493503161,6.51017348825302));
#11603=CARTESIAN_POINT('Ctrl Pts',(-37.7368491027356,32.8418619451291,6.35138876902735));
#11604=CARTESIAN_POINT('Ctrl Pts',(-36.3850216053963,29.6394968734575,6.19260404980166));
#11605=CARTESIAN_POINT('Ctrl Pts',(-38.3426471118536,26.7671664594007,6.03381933057598));
#11606=CARTESIAN_POINT('Ctrl Pts',(-41.8175518092695,26.8544417477417,5.87503461135029));
#11607=CARTESIAN_POINT('Ctrl Pts',(-43.6285178497849,29.8214236540847,5.71624989212461));
#11608=CARTESIAN_POINT('Ctrl Pts',(-42.1176357389792,32.9518892551161,5.55746517289893));
#11609=CARTESIAN_POINT('Ctrl Pts',(-38.6680930907584,33.3799490059277,5.39868045367324));
#11610=CARTESIAN_POINT('Ctrl Pts',(-36.4378892159304,30.7137212758022,5.23989573444757));
#11611=CARTESIAN_POINT('Ctrl Pts',(-37.4687389207455,27.3940935077848,5.08111101522187));
#11612=CARTESIAN_POINT('Ctrl Pts',(-40.81691632925,26.4601300859267,4.92232629599619));
#11613=CARTESIAN_POINT('Ctrl Pts',(-43.4172203331094,28.7668590946468,4.76354157677051));
#11614=CARTESIAN_POINT('Ctrl Pts',(-42.8891155717247,32.2025082317091,4.60475685754482));
#11615=CARTESIAN_POINT('Ctrl Pts',(-39.7160732302253,33.6217974663328,4.44597213831914));
#11616=CARTESIAN_POINT('Ctrl Pts',(-36.802961156292,31.7253909495801,4.28718741909346));
#11617=CARTESIAN_POINT('Ctrl Pts',(-36.8166853311413,28.2494175207298,4.12840269986777));
#11618=CARTESIAN_POINT('Ctrl Pts',(-39.7446814998683,26.3760734330767,3.96961798064209));
#11619=CARTESIAN_POINT('Ctrl Pts',(-42.9064175372036,27.8203742538776,3.81083326141641));
#11620=CARTESIAN_POINT('Ctrl Pts',(-43.407376332096,31.260086438107,3.65204854219072));
#11621=CARTESIAN_POINT('Ctrl Pts',(-40.7889383796118,33.5462103068538,3.49326382296504));
#11622=CARTESIAN_POINT('Ctrl Pts',(-37.4482403780577,32.585837214189,3.33447910373935));
#11623=CARTESIAN_POINT('Ctrl Pts',(-36.4436361477254,29.2581728798308,3.17569438451368));
#11624=CARTESIAN_POINT('Ctrl Pts',(-38.6948242952332,26.6096389957033,3.01690966528799));
#11625=CARTESIAN_POINT('Ctrl Pts',(-42.1408792014373,27.0649246527392,2.85812494606231));
#11626=CARTESIAN_POINT('Ctrl Pts',(-43.6269946413426,30.2072232098169,2.69934022683662));
#11627=CARTESIAN_POINT('Ctrl Pts',(-41.7926562482662,33.15981253181,2.54055550761094));
#11628=CARTESIAN_POINT('Ctrl Pts',(-38.3171709803108,33.2196452983643,2.38177078838525));
#11629=CARTESIAN_POINT('Ctrl Pts',(-36.3822872674944,30.3319467392027,2.22298606915957));
#11630=CARTESIAN_POINT('Ctrl Pts',(-37.7593610245569,27.1403549081105,2.06420134993389));
#11631=CARTESIAN_POINT('Ctrl Pts',(-41.1877003040245,26.566723946295,1.9054166307082));
#11632=CARTESIAN_POINT('Ctrl Pts',(-43.5287244595771,29.1361944527836,1.74663191148252));
#11633=CARTESIAN_POINT('Ctrl Pts',(-42.6392499100348,32.4964767375168,1.58784719225684));
#11634=CARTESIAN_POINT('Ctrl Pts',(-39.3336051438857,33.5712517079766,1.42906247303115));
#11635=CARTESIAN_POINT('Ctrl Pts',(-36.6379949650665,31.3766528609059,1.27027775380547));
#11636=CARTESIAN_POINT('Ctrl Pts',(-37.0203225278291,27.921654956147,1.11149303457979));
#11637=CARTESIAN_POINT('Ctrl Pts',(-40.1303404958339,26.3695395185102,0.952708315354101));
#11638=CARTESIAN_POINT('Ctrl Pts',(-43.1213436114662,28.1406674422797,0.793923596128419));
#11639=CARTESIAN_POINT('Ctrl Pts',(-43.2541897100326,31.6147490004937,0.635138876902735));
#11640=CARTESIAN_POINT('Ctrl Pts',(-40.4091143183855,33.6090247272076,0.476354157677051));
#11641=CARTESIAN_POINT('Ctrl Pts',(-37.1870300541988,32.3023712386336,0.317569438451368));
#11642=CARTESIAN_POINT('Ctrl Pts',(-36.5451700500256,28.8815775163836,0.158784719225683));
#11643=CARTESIAN_POINT('Ctrl Pts',(-38.2187620536724,27.2947612990625,0.0529282397418946));
#11644=CARTESIAN_POINT('Ctrl Pts',(-39.2062007174671,27.0307770462543,0.));
#11645=CARTESIAN_POINT('Ctrl Pts',(-39.2062007174671,27.0307770462543,0.));
#11646=CARTESIAN_POINT('Ctrl Pts',(-39.1131465583677,27.0648166733231,1.22106756688211E-16));
#11647=CARTESIAN_POINT('Ctrl Pts',(-39.0221596232856,27.1036257391105,3.36163846929538E-15));
#11648=CARTESIAN_POINT('Ctrl Pts',(-38.9334476945311,27.1468755170602,3.10862446895044E-15));
#11649=CARTESIAN_POINT('Ctrl Pts',(-38.8427660056612,27.1910856132987,2.84999254446E-15));
#11650=CARTESIAN_POINT('Ctrl Pts',(-38.7544608062646,27.2399364314085,6.47647713978509E-16));
#11651=CARTESIAN_POINT('Ctrl Pts',(-38.6687829655995,27.2931224109893,1.0547118733939E-15));
#11652=CARTESIAN_POINT('Ctrl Pts',(-38.5858335781199,27.3446146567612,1.44881287344555E-15));
#11653=CARTESIAN_POINT('Ctrl Pts',(-38.5053465494816,27.4001712124465,-2.89463008805608E-16));
#11654=CARTESIAN_POINT('Ctrl Pts',(-38.4275832472096,27.4595454790079,-6.10622663543836E-16));
#11655=CARTESIAN_POINT('Ctrl Pts',(-38.3595403577215,27.5114979622491,-8.91637361439786E-16));
#11656=CARTESIAN_POINT('Ctrl Pts',(-38.2935831179973,27.5663740973322,-1.70865430175454E-16));
#11657=CARTESIAN_POINT('Ctrl Pts',(-38.2299118881401,27.6240216579528,-2.77555756156289E-16));
#11658=CARTESIAN_POINT('Ctrl Pts',(-38.2165693475258,27.6361019165031,-2.9991310673269E-16));
#11659=CARTESIAN_POINT('Ctrl Pts',(-38.2033254218291,27.6483057781323,-1.05728990982097E-15));
#11660=CARTESIAN_POINT('Ctrl Pts',(-38.1901991339964,27.6606155381867,-9.99200722162641E-16));
#11661=CARTESIAN_POINT('Ctrl Pts',(-38.1177715281097,27.7285377459838,-6.7867896889854E-16));
#11662=CARTESIAN_POINT('Ctrl Pts',(-38.0488096398962,27.7997811640852,-3.49414594253822E-15));
#11663=CARTESIAN_POINT('Ctrl Pts',(-37.9835528134077,27.8740546235615,-2.692290834716E-15));
#11664=CARTESIAN_POINT('Ctrl Pts',(-37.9186573342444,27.9479168078142,-1.89487584778096E-15));
#11665=CARTESIAN_POINT('Ctrl Pts',(-37.8574255131234,28.024776367863,5.29767817859097E-16));
#11666=CARTESIAN_POINT('Ctrl Pts',(-37.8001363539989,28.1043736902275,1.4432899320127E-15));
#11667=CARTESIAN_POINT('Ctrl Pts',(-37.7442812467117,28.1819785468598,2.33394492634393E-15));
#11668=CARTESIAN_POINT('Ctrl Pts',(-37.6921736179339,28.2621865588976,-1.21793505985174E-15));
#11669=CARTESIAN_POINT('Ctrl Pts',(-37.6441189020832,28.3447712453598,-1.49880108324396E-15));
#11670=CARTESIAN_POINT('Ctrl Pts',(-37.6233913188262,28.3803927433563,-1.61994785897366E-15));
#11671=CARTESIAN_POINT('Ctrl Pts',(-37.6034183971599,28.4164565342063,-1.75461794011481E-15));
#11672=CARTESIAN_POINT('Ctrl Pts',(-37.5842276308026,28.4529447756955,-2.08166817117217E-15));
#11673=CARTESIAN_POINT('Ctrl Pts',(-37.5705623279671,28.47892721228,-2.31455311003352E-15));
#11674=CARTESIAN_POINT('Ctrl Pts',(-37.5572936578702,28.5051248713913,-1.95119937827049E-15));
#11675=CARTESIAN_POINT('Ctrl Pts',(-37.5444321439544,28.531531314607,-2.13717932240343E-15));
#11676=CARTESIAN_POINT('Ctrl Pts',(-37.538816666632,28.543060655866,-2.21838019545243E-15));
#11677=CARTESIAN_POINT('Ctrl Pts',(-37.5332797327988,28.5546280003926,3.28930239803853E-15));
#11678=CARTESIAN_POINT('Ctrl Pts',(-37.5278259127264,28.5662245354477,3.1641356201817E-15));
#11679=CARTESIAN_POINT('Ctrl Pts',(-37.4875980549542,28.6517616005977,2.24089442948892E-15));
#11680=CARTESIAN_POINT('Ctrl Pts',(-37.4518262344481,28.7390118083874,-3.58197140345829E-15));
#11681=CARTESIAN_POINT('Ctrl Pts',(-37.4207614303772,28.8277378411266,-3.21964677141295E-15));
#11682=CARTESIAN_POINT('Ctrl Pts',(-37.3903833360849,28.9145025212636,-2.86533158527601E-15));
#11683=CARTESIAN_POINT('Ctrl Pts',(-37.3645062370121,29.0026791737866,-9.81657689619027E-16));
#11684=CARTESIAN_POINT('Ctrl Pts',(-37.3434139515882,29.0920546900511,2.77555756156289E-16));
#11685=CARTESIAN_POINT('Ctrl Pts',(-37.3396852215853,29.1078546454526,5.00161645507665E-16));
#11686=CARTESIAN_POINT('Ctrl Pts',(-37.3361061566853,29.1236920756746,-4.14690112491889E-16));
#11687=CARTESIAN_POINT('Ctrl Pts',(-37.3326784971319,29.1395658089505,-4.16333634234434E-16));
#11688=CARTESIAN_POINT('Ctrl Pts',(-37.3125675986992,29.2327007987852,-3.98220993782475E-16));
#11689=CARTESIAN_POINT('Ctrl Pts',(-37.2976646715474,29.3270865450837,4.99300212322796E-16));
#11690=CARTESIAN_POINT('Ctrl Pts',(-37.2878912238873,29.4223141487873,1.16573417585641E-15));
#11691=CARTESIAN_POINT('Ctrl Pts',(-37.2846133376322,29.4542522390242,1.38924739299596E-15));
#11692=CARTESIAN_POINT('Ctrl Pts',(-37.2819128543797,29.486284903846,-3.05311331771918E-16));
#11693=CARTESIAN_POINT('Ctrl Pts',(-37.279788037766,29.5183962478047,-3.05311331771918E-16));
#11694=CARTESIAN_POINT('Ctrl Pts',(-37.2785994180604,29.5363592926898,-3.05311331771918E-16));
#11695=CARTESIAN_POINT('Ctrl Pts',(-37.2775909505956,29.5543469531232,1.33873046221551E-15));
#11696=CARTESIAN_POINT('Ctrl Pts',(-37.2767624107733,29.5723564016008,1.38777878078145E-15));
#11697=CARTESIAN_POINT('Ctrl Pts',(-37.2761881456715,29.584838840566,1.42177441610613E-15));
#11698=CARTESIAN_POINT('Ctrl Pts',(-37.2757004320392,29.5973302169591,1.41595233551992E-15));
#11699=CARTESIAN_POINT('Ctrl Pts',(-37.2752993200193,29.6098201091207,1.41553435639707E-15));
#11700=CARTESIAN_POINT('Ctrl Pts',(-37.2723065021044,29.7030109664475,1.41241568793312E-15));
#11701=CARTESIAN_POINT('Ctrl Pts',(-37.2741232733776,29.7962662842263,3.40525005655215E-15));
#11702=CARTESIAN_POINT('Ctrl Pts',(-37.2806105303684,29.8892109312269,3.67761376907083E-15));
#11703=CARTESIAN_POINT('Ctrl Pts',(-37.2871107458397,29.9823412378062,3.95052153586022E-15));
#11704=CARTESIAN_POINT('Ctrl Pts',(-37.2983005079771,30.0751606128563,7.05637141741307E-16));
#11705=CARTESIAN_POINT('Ctrl Pts',(-37.3140909235774,30.1672796708414,1.22124532708767E-15));
#11706=CARTESIAN_POINT('Ctrl Pts',(-37.32965822843,30.2580971321851,1.72956822427593E-15));
#11707=CARTESIAN_POINT('Ctrl Pts',(-37.349697563177,30.3482347740108,1.91557599461872E-15));
#11708=CARTESIAN_POINT('Ctrl Pts',(-37.374166796696,30.4372943327761,1.84574577843932E-15));
#11709=CARTESIAN_POINT('Ctrl Pts',(-37.3836804577095,30.4719207730141,1.81859572469031E-15));
#11710=CARTESIAN_POINT('Ctrl Pts',(-37.3938641977425,30.506383904736,1.42353668742041E-15));
#11711=CARTESIAN_POINT('Ctrl Pts',(-37.4047171072924,30.5406588580658,1.06858966120171E-15));
#11712=CARTESIAN_POINT('Ctrl Pts',(-37.4105213261189,30.5589893645979,8.78761283608898E-16));
#11713=CARTESIAN_POINT('Ctrl Pts',(-37.4165169545494,30.5772660329217,4.70005909401713E-15));
#11714=CARTESIAN_POINT('Ctrl Pts',(-37.4227039491659,30.5954849444668,4.92661467177413E-15));
#11715=CARTESIAN_POINT('Ctrl Pts',(-37.4281525600734,30.6115295293288,5.12613208994136E-15));
#11716=CARTESIAN_POINT('Ctrl Pts',(-37.433750064935,30.6275303950272,2.76438724788175E-15));
#11717=CARTESIAN_POINT('Ctrl Pts',(-37.4394903125654,30.6434684551818,2.87270207621759E-15));
#11718=CARTESIAN_POINT('Ctrl Pts',(-37.4719158032,30.7334993133521,3.48455049773622E-15));
#11719=CARTESIAN_POINT('Ctrl Pts',(-37.5089323379402,30.821651437624,4.98050361397802E-15));
#11720=CARTESIAN_POINT('Ctrl Pts',(-37.5504668820251,30.9074802563227,5.40539835114373E-15));
#11721=CARTESIAN_POINT('Ctrl Pts',(-37.5816177900888,30.9718518703467,5.72406940401801E-15));
#11722=CARTESIAN_POINT('Ctrl Pts',(-37.6153112267555,31.0349160880258,2.99557423021898E-15));
#11723=CARTESIAN_POINT('Ctrl Pts',(-37.6515337488198,31.0964681987463,3.17801340798951E-15));
#11724=CARTESIAN_POINT('Ctrl Pts',(-37.6664655212945,31.1218414212673,3.2532191125533E-15));
#11725=CARTESIAN_POINT('Ctrl Pts',(-37.6818272197272,31.1469574944417,2.59709908762232E-15));
#11726=CARTESIAN_POINT('Ctrl Pts',(-37.6976185603144,31.1718011729578,2.26901830657766E-15));
#11727=CARTESIAN_POINT('Ctrl Pts',(-37.7070512127228,31.18664106465,2.07304558644154E-15));
#11728=CARTESIAN_POINT('Ctrl Pts',(-37.7166324846138,31.2013763450879,7.23090290612832E-15));
#11729=CARTESIAN_POINT('Ctrl Pts',(-37.7263603370399,31.2160016924469,6.80011602582908E-15));
#11730=CARTESIAN_POINT('Ctrl Pts',(-37.7738890060192,31.2874587070981,4.69536297885029E-15));
#11731=CARTESIAN_POINT('Ctrl Pts',(-37.8249264593017,31.3563137429908,3.52571416788317E-15));
#11732=CARTESIAN_POINT('Ctrl Pts',(-37.879438314505,31.4222140867493,2.82412981889024E-15));
#11733=CARTESIAN_POINT('Ctrl Pts',(-37.9310243832669,31.4845773956458,2.16020124162171E-15));
#11734=CARTESIAN_POINT('Ctrl Pts',(-37.9857223942837,31.544294891251,2.53051231403829E-15));
#11735=CARTESIAN_POINT('Ctrl Pts',(-38.0435270002979,31.6010317842403,2.43164863245049E-15));
#11736=CARTESIAN_POINT('Ctrl Pts',(-38.0564929750925,31.6137582635843,2.39949816171156E-15));
#11737=CARTESIAN_POINT('Ctrl Pts',(-38.0696153396013,31.6263346192956,-2.49073063447215E-17));
#11738=CARTESIAN_POINT('Ctrl Pts',(-38.0828908636835,31.6387595214235,-2.77555756156289E-17));
#11739=CARTESIAN_POINT('Ctrl Pts',(-42.5194677947045,29.9980220285566,8.38741669750802));
#11740=CARTESIAN_POINT('Ctrl Pts',(-42.5205892939538,29.8678903777981,8.3956620675864));
#11741=CARTESIAN_POINT('Ctrl Pts',(-42.5113777972944,29.7379179862643,8.40390743766478));
#11742=CARTESIAN_POINT('Ctrl Pts',(-42.4912802970509,29.6096514007085,8.41215280774316));
#11743=CARTESIAN_POINT('Ctrl Pts',(-42.3622714956278,28.7862893773384,8.46508104748506));
#11744=CARTESIAN_POINT('Ctrl Pts',(-41.7847000858182,28.0332158462492,8.51800928722695));
#11745=CARTESIAN_POINT('Ctrl Pts',(-41.0229436280752,27.6951313564435,8.57093752696884));
#11746=CARTESIAN_POINT('Ctrl Pts',(-40.2611871703322,27.3570468666378,8.62386576671074));
#11747=CARTESIAN_POINT('Ctrl Pts',(-39.3152456646558,27.4339514181157,8.67679400645263));
#11748=CARTESIAN_POINT('Ctrl Pts',(-38.6181179828953,27.890667827996,8.72972224619453));
#11749=CARTESIAN_POINT('Ctrl Pts',(-37.9209903011348,28.3473842378763,8.78265048593642));
#11750=CARTESIAN_POINT('Ctrl Pts',(-37.4726764432901,29.1839125061591,8.83557872567832));
#11751=CARTESIAN_POINT('Ctrl Pts',(-37.4783844595774,30.0172883248844,8.88850696542021));
#11752=CARTESIAN_POINT('Ctrl Pts',(-37.4840924758647,30.8506641436097,8.9414352051621));
#11753=CARTESIAN_POINT('Ctrl Pts',(-37.9438223662839,31.6808875127775,8.994363444904));
#11754=CARTESIAN_POINT('Ctrl Pts',(-38.6471443887468,32.1280311923952,9.0472916846459));
#11755=CARTESIAN_POINT('Ctrl Pts',(-39.3504664112097,32.575174872013,9.10021992438779));
#11756=CARTESIAN_POINT('Ctrl Pts',(-40.2973805657162,32.6392388620807,9.15314816412969));
#11757=CARTESIAN_POINT('Ctrl Pts',(-41.0544291129542,32.2906973974148,9.20607640387158));
#11758=CARTESIAN_POINT('Ctrl Pts',(-41.8114776601922,31.9421559327489,9.25900464361347));
#11759=CARTESIAN_POINT('Ctrl Pts',(-42.3786606001618,31.1810090133494,9.31193288335537));
#11760=CARTESIAN_POINT('Ctrl Pts',(-42.4963857173162,30.356066933708,9.36486112309726));
#11761=CARTESIAN_POINT('Ctrl Pts',(-42.5131087222309,30.2388828460158,9.37237964790084));
#11762=CARTESIAN_POINT('Ctrl Pts',(-42.5207623112886,30.1204114632572,9.37989817270443));
#11763=CARTESIAN_POINT('Ctrl Pts',(-42.5197815649842,30.0018165623494,9.38741669750802));
#11764=CARTESIAN_POINT('Ctrl Pts',(-40.7937992825329,27.0307770462543,10.));
#11765=CARTESIAN_POINT('Ctrl Pts',(-41.7812379463276,27.2947612990625,9.94707176025811));
#11766=CARTESIAN_POINT('Ctrl Pts',(-43.4548297940574,28.8815785121496,9.84121528077431));
#11767=CARTESIAN_POINT('Ctrl Pts',(-42.8129700816392,32.3023708276668,9.68243056154864));
#11768=CARTESIAN_POINT('Ctrl Pts',(-39.5908856649077,33.609025071703,9.52364584232295));
#11769=CARTESIAN_POINT('Ctrl Pts',(-36.7458102038522,31.6147488878258,9.36486112309727));
#11770=CARTESIAN_POINT('Ctrl Pts',(-36.8786563309339,28.140667484321,9.20607640387158));
#11771=CARTESIAN_POINT('Ctrl Pts',(-39.869659490377,26.3695393883571,9.0472916846459));
#11772=CARTESIAN_POINT('Ctrl Pts',(-42.9796775476457,27.9216549347271,8.88850696542022));
#11773=CARTESIAN_POINT('Ctrl Pts',(-43.3620051070722,31.3766528780855,8.72972224619453));
#11774=CARTESIAN_POINT('Ctrl Pts',(-40.6663948741839,33.5712517973455,8.57093752696885));
#11775=CARTESIAN_POINT('Ctrl Pts',(-37.3607500279849,32.4964767903705,8.41215280774316));
#11776=CARTESIAN_POINT('Ctrl Pts',(-36.4712754607486,29.1361944352982,8.25336808851748));
#11777=CARTESIAN_POINT('Ctrl Pts',(-38.812299668292,26.5667238666358,8.0945833692918));
#11778=CARTESIAN_POINT('Ctrl Pts',(-42.2406390269471,27.1403548434066,7.93579865006611));
#11779=CARTESIAN_POINT('Ctrl Pts',(-43.6177128150067,30.3319467464472,7.77701393084043));
#11780=CARTESIAN_POINT('Ctrl Pts',(-41.6828290582353,33.2196453721168,7.61822921161475));
#11781=CARTESIAN_POINT('Ctrl Pts',(-38.20734371072,33.1598126039199,7.45944449238906));
#11782=CARTESIAN_POINT('Ctrl Pts',(-36.3730052758037,30.2072232146022,7.30065977316339));
#11783=CARTESIAN_POINT('Ctrl Pts',(-37.859120749627,27.0649245856435,7.14187505393769));
#11784=CARTESIAN_POINT('Ctrl Pts',(-41.305175734599,26.6096389182437,6.98309033471202));
#11785=CARTESIAN_POINT('Ctrl Pts',(-43.5563639335371,29.258172862872,6.82430561548633));
#11786=CARTESIAN_POINT('Ctrl Pts',(-42.551759680255,32.5858372732818,6.66552089626064));
#11787=CARTESIAN_POINT('Ctrl Pts',(-39.211061602359,33.5462103878864,6.50673617703497));
#11788=CARTESIAN_POINT('Ctrl Pts',(-36.5926235900426,31.2600864669024,6.34795145780927));
#11789=CARTESIAN_POINT('Ctrl Pts',(-37.0935823963814,27.8203742040704,6.1891667385836));
#11790=CARTESIAN_POINT('Ctrl Pts',(-40.2553185059661,26.3760733502665,6.0303820193579));
#11791=CARTESIAN_POINT('Ctrl Pts',(-43.1833147416005,28.249417480727,5.87159730013223));
#11792=CARTESIAN_POINT('Ctrl Pts',(-43.1970389167639,31.7253909890071,5.71281258090654));
#11793=CARTESIAN_POINT('Ctrl Pts',(-40.2839267762627,33.6217975490946,5.55402786168086));
#11794=CARTESIAN_POINT('Ctrl Pts',(-37.1108843622561,32.2025082820388,5.39524314245517));
#11795=CARTESIAN_POINT('Ctrl Pts',(-36.5827795888035,28.7668590664683,5.2364584232295));
#11796=CARTESIAN_POINT('Ctrl Pts',(-39.1830836520825,26.460130005037,5.07767370400381));
#11797=CARTESIAN_POINT('Ctrl Pts',(-42.5312611370964,27.3940934482371,4.91888898477813));
#11798=CARTESIAN_POINT('Ctrl Pts',(-43.5621108654676,30.7137212921113,4.76010426555244));
#11799=CARTESIAN_POINT('Ctrl Pts',(-41.331906939677,33.379949083163,4.60131954632676));
#11800=CARTESIAN_POINT('Ctrl Pts',(-37.8823642126307,32.9518893225699,4.44253482710107));
#11801=CARTESIAN_POINT('Ctrl Pts',(-36.3714820672996,29.821423650004,4.2837501078754));
#11802=CARTESIAN_POINT('Ctrl Pts',(-38.1824481491975,26.8544416758625,4.1249653886497));
#11803=CARTESIAN_POINT('Ctrl Pts',(-41.6573529260186,26.767166385527,3.96618066942403));
#11804=CARTESIAN_POINT('Ctrl Pts',(-43.6149784772097,29.6394968652198,3.80739595019834));
#11805=CARTESIAN_POINT('Ctrl Pts',(-42.2631509489798,32.8418620100683,3.64861123097266));
#11806=CARTESIAN_POINT('Ctrl Pts',(-38.8394461124454,33.4425494289825,3.48982651174697));
#11807=CARTESIAN_POINT('Ctrl Pts',(-36.4782091884119,30.8916397157027,3.33104179252129));
#11808=CARTESIAN_POINT('Ctrl Pts',(-37.3411135755689,27.5244485680153,3.17225707329561));
#11809=CARTESIAN_POINT('Ctrl Pts',(-40.6381845610556,26.4235838698918,3.01347235406992));
#11810=CARTESIAN_POINT('Ctrl Pts',(-43.3510081243786,28.5968690440692,2.85468763484424));
#11811=CARTESIAN_POINT('Ctrl Pts',(-42.9960391033767,32.0546974604333,2.69590291561856));
#11812=CARTESIAN_POINT('Ctrl Pts',(-39.8982457801193,33.6314842325659,2.53711819639287));
#11813=CARTESIAN_POINT('Ctrl Pts',(-36.893606754763,31.8837073010328,2.37833347716719));
#11814=CARTESIAN_POINT('Ctrl Pts',(-36.7328194493102,28.4114272089134,2.21954875794151));
#11815=CARTESIAN_POINT('Ctrl Pts',(-39.5630819289538,26.3934597519746,2.06076403871582));
#11816=CARTESIAN_POINT('Ctrl Pts',(-42.7933357607888,27.6772193427188,1.90197931949014));
#11817=CARTESIAN_POINT('Ctrl Pts',(-43.4663366961235,31.0874481963816,1.74319460026445));
#11818=CARTESIAN_POINT('Ctrl Pts',(-40.9659639490253,33.5021323126134,1.58440988103877));
#11819=CARTESIAN_POINT('Ctrl Pts',(-37.5812665608262,32.7106798921575,1.42562516181309));
#11820=CARTESIAN_POINT('Ctrl Pts',(-36.4108808842817,29.4376293456934,1.2668404425874));
#11821=CARTESIAN_POINT('Ctrl Pts',(-38.5262720652766,26.679450722727,1.10805572336172));
#11822=CARTESIAN_POINT('Ctrl Pts',(-41.9908416256376,26.9611184445014,0.949271004136038));
#11823=CARTESIAN_POINT('Ctrl Pts',(-43.6328189794496,30.024955176587,0.790486284910354));
#11824=CARTESIAN_POINT('Ctrl Pts',(-41.9490297104332,33.065699934597,0.63170156568467));
#11825=CARTESIAN_POINT('Ctrl Pts',(-38.4808977151712,33.3003381572967,0.472916846458986));
#11826=CARTESIAN_POINT('Ctrl Pts',(-36.4035550591505,30.5125904676491,0.314132127233303));
#11827=CARTESIAN_POINT('Ctrl Pts',(-37.6185464810465,27.2575347505532,0.155347408007618));
#11828=CARTESIAN_POINT('Ctrl Pts',(-41.0140157220173,26.5092287064619,-0.00343731121806403));
#11829=CARTESIAN_POINT('Ctrl Pts',(-43.4806523136791,28.9647343328049,-0.162222030443749));
#11830=CARTESIAN_POINT('Ctrl Pts',(-43.0002811455948,31.2204253757916,-0.268078509927538));
#11831=CARTESIAN_POINT('Ctrl Pts',(-42.3360626576962,31.9973015569307,-0.321006749669432));
#11832=CARTESIAN_POINT('Ctrl Pts',(-40.7459328543469,27.2098224301578,10.1070022498898));
#11833=CARTESIAN_POINT('Ctrl Pts',(-41.673828554412,27.4578883222956,10.0540740101479));
#11834=CARTESIAN_POINT('Ctrl Pts',(-43.246502114919,28.9490197948615,9.94821753066413));
#11835=CARTESIAN_POINT('Ctrl Pts',(-42.6433468111667,32.1635369054084,9.78943281143844));
#11836=CARTESIAN_POINT('Ctrl Pts',(-39.6155554301386,33.3913993529387,9.63064809221277));
#11837=CARTESIAN_POINT('Ctrl Pts',(-36.9420392073399,31.5173788556549,9.47186337298707));
#11838=CARTESIAN_POINT('Ctrl Pts',(-37.0668746574889,28.2527860113768,9.3130786537614));
#11839=CARTESIAN_POINT('Ctrl Pts',(-39.8775190775307,26.5884576791301,9.1542939345357));
#11840=CARTESIAN_POINT('Ctrl Pts',(-42.8000017473647,28.0469800099716,8.99550921531003));
#11841=CARTESIAN_POINT('Ctrl Pts',(-43.1592747953177,31.2936401347184,8.83672449608433));
#11842=CARTESIAN_POINT('Ctrl Pts',(-40.6262109850188,33.3559038227971,8.67793977685867));
#11843=CARTESIAN_POINT('Ctrl Pts',(-37.5198979033106,32.3459381975126,8.51915505763297));
#11844=CARTESIAN_POINT('Ctrl Pts',(-36.6840590238768,29.1882822715299,8.36037033840731));
#11845=CARTESIAN_POINT('Ctrl Pts',(-38.8839184942158,26.7737518510347,8.20158561918159));
#11846=CARTESIAN_POINT('Ctrl Pts',(-42.1055275580482,27.312792640388,8.04280089995594));
#11847=CARTESIAN_POINT('Ctrl Pts',(-43.3995632216936,30.3119302190328,7.88401618073023));
#11848=CARTESIAN_POINT('Ctrl Pts',(-41.581353763362,33.0254994118221,7.72523146150456));
#11849=CARTESIAN_POINT('Ctrl Pts',(-38.3154416334834,32.9692745845306,7.56644674227887));
#11850=CARTESIAN_POINT('Ctrl Pts',(-36.5917145721166,30.1947275682361,7.4076620230532));
#11851=CARTESIAN_POINT('Ctrl Pts',(-37.988216662344,27.2419108586636,7.2488773038275));
#11852=CARTESIAN_POINT('Ctrl Pts',(-41.2264730928294,26.8140791071116,7.09009258460183));
#11853=CARTESIAN_POINT('Ctrl Pts',(-43.3419137033927,29.3029053489892,6.93130786537614));
#11854=CARTESIAN_POINT('Ctrl Pts',(-42.3978875060538,32.4299102059921,6.77252314615045));
#11855=CARTESIAN_POINT('Ctrl Pts',(-39.2586349171563,33.3323724207843,6.61373842692477));
#11856=CARTESIAN_POINT('Ctrl Pts',(-36.7980898103057,31.1841027268018,6.45495370769909));
#11857=CARTESIAN_POINT('Ctrl Pts',(-37.268840591448,27.951806549663,6.29616898847341));
#11858=CARTESIAN_POINT('Ctrl Pts',(-40.2399226934486,26.5945976404082,6.13738426924772));
#11859=CARTESIAN_POINT('Ctrl Pts',(-42.9913595334959,28.3549783375912,5.97859955002203));
#11860=CARTESIAN_POINT('Ctrl Pts',(-43.0042561351662,31.6213491919367,5.81981483079636));
#11861=CARTESIAN_POINT('Ctrl Pts',(-40.2668058731011,33.4034016446103,5.66103011157067));
#11862=CARTESIAN_POINT('Ctrl Pts',(-37.2850992415561,32.0696961129792,5.50224539234499));
#11863=CARTESIAN_POINT('Ctrl Pts',(-36.7888394064517,28.8412179796556,5.3434606731193));
#11864=CARTESIAN_POINT('Ctrl Pts',(-39.2323440489636,26.6735856437984,5.18467595389362));
#11865=CARTESIAN_POINT('Ctrl Pts',(-42.3786250336068,27.5512307013991,5.02589123466794));
#11866=CARTESIAN_POINT('Ctrl Pts',(-43.3473140929281,30.6706836001842,4.86710651544225));
#11867=CARTESIAN_POINT('Ctrl Pts',(-41.2515923950797,33.1761367421578,4.70832179621657));
#11868=CARTESIAN_POINT('Ctrl Pts',(-38.0100585348234,32.7738891638639,4.54953707699088));
#11869=CARTESIAN_POINT('Ctrl Pts',(-36.5902832137214,29.8321918784729,4.39075235776521));
#11870=CARTESIAN_POINT('Ctrl Pts',(-38.2920472847157,27.0441201562291,4.23196763853951));
#11871=CARTESIAN_POINT('Ctrl Pts',(-41.5574138525555,26.9621076023424,4.07318291931384));
#11872=CARTESIAN_POINT('Ctrl Pts',(-43.3969937656074,29.6612353547743,3.91439820008815));
#11873=CARTESIAN_POINT('Ctrl Pts',(-42.1266820017825,32.6704965442478,3.75561348086247));
#11874=CARTESIAN_POINT('Ctrl Pts',(-38.9094279964517,33.2349622609857,3.59682876163679));
#11875=CARTESIAN_POINT('Ctrl Pts',(-36.6905746448669,30.8378734685435,3.4380440424111));
#11876=CARTESIAN_POINT('Ctrl Pts',(-37.5014455371744,27.6737253530252,3.27925932318542));
#11877=CARTESIAN_POINT('Ctrl Pts',(-40.5997017655514,26.6392432558621,3.12047460395973));
#11878=CARTESIAN_POINT('Ctrl Pts',(-43.1489409352723,28.6814784265862,2.96168988473405));
#11879=CARTESIAN_POINT('Ctrl Pts',(-42.8153766944534,31.9307983456346,2.80290516550837));
#11880=CARTESIAN_POINT('Ctrl Pts',(-39.9043816020653,33.4125042170238,2.64412044628269));
#11881=CARTESIAN_POINT('Ctrl Pts',(-37.0809235645186,31.7701189642425,2.485335727057));
#11882=CARTESIAN_POINT('Ctrl Pts',(-36.929831800721,28.5072188115211,2.32655100783132));
#11883=CARTESIAN_POINT('Ctrl Pts',(-39.5894282710721,26.6109356348337,2.16776628860563));
#11884=CARTESIAN_POINT('Ctrl Pts',(-42.6248964480619,27.817283986225,2.00898156937995));
#11885=CARTESIAN_POINT('Ctrl Pts',(-43.2573151459858,31.0218746160781,1.85019685015426));
#11886=CARTESIAN_POINT('Ctrl Pts',(-40.9077159195629,33.290952271855,1.69141213092858));
#11887=CARTESIAN_POINT('Ctrl Pts',(-37.7271171971453,32.5472247628218,1.5326274117029));
#11888=CARTESIAN_POINT('Ctrl Pts',(-36.6273062655885,29.4715405309648,1.37384269247722));
#11889=CARTESIAN_POINT('Ctrl Pts',(-38.6151384750923,26.8796812306348,1.21505797325153));
#11890=CARTESIAN_POINT('Ctrl Pts',(-41.8707930443401,27.1443642711765,1.05627325402585));
#11891=CARTESIAN_POINT('Ctrl Pts',(-43.413758478113,30.0234503690188,0.897488534800164));
#11892=CARTESIAN_POINT('Ctrl Pts',(-41.831502405081,32.8808369484644,0.738703815574481));
#11893=CARTESIAN_POINT('Ctrl Pts',(-38.5725002172442,33.1013263883626,0.579919096348796));
#11894=CARTESIAN_POINT('Ctrl Pts',(-36.6204221907717,30.4816810484188,0.421134377123114));
#11895=CARTESIAN_POINT('Ctrl Pts',(-37.7621491226102,27.4229065502053,0.262349657897428));
#11896=CARTESIAN_POINT('Ctrl Pts',(-40.9528701505796,26.7197236730263,0.103564938671747));
#11897=CARTESIAN_POINT('Ctrl Pts',(-43.2707675258253,29.0271612848097,-0.0552197805539385));
#11898=CARTESIAN_POINT('Ctrl Pts',(-42.8193629397544,31.1468332160454,-0.161076260037727));
#11899=CARTESIAN_POINT('Ctrl Pts',(-42.1951971040191,31.8768634390788,-0.214004499779622));
#11900=CARTESIAN_POINT('Ctrl Pts',(-40.698066426161,27.3888678140614,10.2140044997796));
#11901=CARTESIAN_POINT('Ctrl Pts',(-41.5664191624963,27.6210153455288,10.1610762600377));
#11902=CARTESIAN_POINT('Ctrl Pts',(-43.0381744357806,29.0164610775733,10.0552197805539));
#11903=CARTESIAN_POINT('Ctrl Pts',(-42.4737235406942,32.0247029831501,9.89643506132824));
#11904=CARTESIAN_POINT('Ctrl Pts',(-39.6402251953695,33.1737736341743,9.73765034210259));
#11905=CARTESIAN_POINT('Ctrl Pts',(-37.1382682108276,31.4200088234841,9.57886562287687));
#11906=CARTESIAN_POINT('Ctrl Pts',(-37.2550929840439,28.3649045384325,9.42008090365121));
#11907=CARTESIAN_POINT('Ctrl Pts',(-39.8853786646844,26.8073759699033,9.26129618442551));
#11908=CARTESIAN_POINT('Ctrl Pts',(-42.6203259470837,28.172305085216,9.10251146519984));
#11909=CARTESIAN_POINT('Ctrl Pts',(-42.9565444835633,31.2106273913515,8.94372674597415));
#11910=CARTESIAN_POINT('Ctrl Pts',(-40.5860270958538,33.1405558482486,8.78494202674847));
#11911=CARTESIAN_POINT('Ctrl Pts',(-37.6790457786362,32.1953996046547,8.62615730752278));
#11912=CARTESIAN_POINT('Ctrl Pts',(-36.896842587005,29.2403701077616,8.46737258829711));
#11913=CARTESIAN_POINT('Ctrl Pts',(-38.9555373201395,26.9807798354337,8.30858786907141));
#11914=CARTESIAN_POINT('Ctrl Pts',(-41.9704160891492,27.4852304373692,8.14980314984574));
#11915=CARTESIAN_POINT('Ctrl Pts',(-43.1814136283805,30.2919136916184,7.99101843062005));
#11916=CARTESIAN_POINT('Ctrl Pts',(-41.4798784684888,32.8313534515275,7.83223371139437));
#11917=CARTESIAN_POINT('Ctrl Pts',(-38.4235395562468,32.7787365651412,7.67344899216869));
#11918=CARTESIAN_POINT('Ctrl Pts',(-36.8104238684295,30.18223192187,7.514664272943));
#11919=CARTESIAN_POINT('Ctrl Pts',(-38.117312575061,27.4188971316837,7.35587955371732));
#11920=CARTESIAN_POINT('Ctrl Pts',(-41.1477704510597,27.0185192959796,7.19709483449164));
#11921=CARTESIAN_POINT('Ctrl Pts',(-43.1274634732482,29.3476378351063,7.03831011526595));
#11922=CARTESIAN_POINT('Ctrl Pts',(-42.2440153318527,32.2739831387024,6.87952539604027));
#11923=CARTESIAN_POINT('Ctrl Pts',(-39.3062082319536,33.1185344536822,6.72074067681459));
#11924=CARTESIAN_POINT('Ctrl Pts',(-37.0035560305689,31.1081189867012,6.5619559575889));
#11925=CARTESIAN_POINT('Ctrl Pts',(-37.4440987865146,28.0832388952556,6.40317123836322));
#11926=CARTESIAN_POINT('Ctrl Pts',(-40.2245268809313,26.81312193055,6.24438651913753));
#11927=CARTESIAN_POINT('Ctrl Pts',(-42.7994043253911,28.4605391944553,6.08560179991184));
#11928=CARTESIAN_POINT('Ctrl Pts',(-42.8114733535686,31.5173073948663,5.92681708068617));
#11929=CARTESIAN_POINT('Ctrl Pts',(-40.2496849699394,33.1850057401262,5.76803236146048));
#11930=CARTESIAN_POINT('Ctrl Pts',(-37.4593141208561,31.9368839439196,5.6092476422348));
#11931=CARTESIAN_POINT('Ctrl Pts',(-36.9948992240999,28.9155768928429,5.45046292300912));
#11932=CARTESIAN_POINT('Ctrl Pts',(-39.2816044458447,26.8870412825597,5.29167820378343));
#11933=CARTESIAN_POINT('Ctrl Pts',(-42.2259889301172,27.7083679545611,5.13289348455775));
#11934=CARTESIAN_POINT('Ctrl Pts',(-43.1325173203886,30.6276459082571,4.97410876533206));
#11935=CARTESIAN_POINT('Ctrl Pts',(-41.1712778504822,32.9723244011526,4.81532404610638));
#11936=CARTESIAN_POINT('Ctrl Pts',(-38.137752857016,32.5958890051579,4.6565393268807));
#11937=CARTESIAN_POINT('Ctrl Pts',(-36.8090843601431,29.8429601069419,4.49775460765501));
#11938=CARTESIAN_POINT('Ctrl Pts',(-38.401646420234,27.2337986365958,4.33896988842933));
#11939=CARTESIAN_POINT('Ctrl Pts',(-41.4574747790924,27.1570488191579,4.18018516920364));
#11940=CARTESIAN_POINT('Ctrl Pts',(-43.1790090540052,29.6829738443289,4.02140044997797));
#11941=CARTESIAN_POINT('Ctrl Pts',(-41.9902130545851,32.4991310784273,3.86261573075228));
#11942=CARTESIAN_POINT('Ctrl Pts',(-38.9794098804581,33.027375092989,3.7038310115266));
#11943=CARTESIAN_POINT('Ctrl Pts',(-36.9029401013218,30.7841072213844,3.54504629230091));
#11944=CARTESIAN_POINT('Ctrl Pts',(-37.66177749878,27.823002138035,3.38626157307523));
#11945=CARTESIAN_POINT('Ctrl Pts',(-40.5612189700471,26.8549026418326,3.22747685384954));
#11946=CARTESIAN_POINT('Ctrl Pts',(-42.946873746166,28.7660878091031,3.06869213462386));
#11947=CARTESIAN_POINT('Ctrl Pts',(-42.6347142855301,31.806899230836,2.90990741539817));
#11948=CARTESIAN_POINT('Ctrl Pts',(-39.9105174240114,33.1935242014816,2.7511226961725));
#11949=CARTESIAN_POINT('Ctrl Pts',(-37.2682403742742,31.6565306274523,2.59233797694681));
#11950=CARTESIAN_POINT('Ctrl Pts',(-37.1268441521318,28.6030104141288,2.43355325772113));
#11951=CARTESIAN_POINT('Ctrl Pts',(-39.6157746131904,26.8284115176927,2.27476853849544));
#11952=CARTESIAN_POINT('Ctrl Pts',(-42.456457135335,27.9573486297311,2.11598381926976));
#11953=CARTESIAN_POINT('Ctrl Pts',(-43.0482935958481,30.9563010357746,1.95719910004407));
#11954=CARTESIAN_POINT('Ctrl Pts',(-40.8494678901005,33.0797722310966,1.79841438081839));
#11955=CARTESIAN_POINT('Ctrl Pts',(-37.8729678334645,32.3837696334862,1.63962966159271));
#11956=CARTESIAN_POINT('Ctrl Pts',(-36.8437316468953,29.5054517162361,1.48084494236703));
#11957=CARTESIAN_POINT('Ctrl Pts',(-38.7040048849081,27.0799117385426,1.32206022314134));
#11958=CARTESIAN_POINT('Ctrl Pts',(-41.7507444630425,27.3276100978515,1.16327550391566));
#11959=CARTESIAN_POINT('Ctrl Pts',(-43.1946979767764,30.0219455614506,1.00449078468998));
#11960=CARTESIAN_POINT('Ctrl Pts',(-41.7139750997287,32.6959739623317,0.84570606546429));
#11961=CARTESIAN_POINT('Ctrl Pts',(-38.6641027193173,32.9023146194285,0.686921346238608));
#11962=CARTESIAN_POINT('Ctrl Pts',(-36.8372893223927,30.4507716291885,0.528136627012924));
#11963=CARTESIAN_POINT('Ctrl Pts',(-37.9057517641739,27.5882783498574,0.369351907787239));
#11964=CARTESIAN_POINT('Ctrl Pts',(-40.8917245791419,26.9302186395907,0.210567188561557));
#11965=CARTESIAN_POINT('Ctrl Pts',(-43.0608827379715,29.0895882368145,0.0517824693358725));
#11966=CARTESIAN_POINT('Ctrl Pts',(-42.6384447339141,31.0732410562992,-0.0540740101479163));
#11967=CARTESIAN_POINT('Ctrl Pts',(-42.0543315503421,31.7564253212269,-0.107002249889811));
#11968=CARTESIAN_POINT('Ctrl Pts',(-40.6501999979751,27.5679131979649,10.3210067496694));
#11969=CARTESIAN_POINT('Ctrl Pts',(-41.4590097705807,27.7841423687619,10.2680785099275));
#11970=CARTESIAN_POINT('Ctrl Pts',(-42.8298467566421,29.0839023602852,10.1622220304438));
#11971=CARTESIAN_POINT('Ctrl Pts',(-42.3041002702218,31.8858690608918,10.0034373112181));
#11972=CARTESIAN_POINT('Ctrl Pts',(-39.6648949606003,32.95614791541,9.8446525919924));
#11973=CARTESIAN_POINT('Ctrl Pts',(-37.3344972143153,31.3226387913133,9.68586787276669));
#11974=CARTESIAN_POINT('Ctrl Pts',(-37.443311310599,28.4770230654882,9.52708315354102));
#11975=CARTESIAN_POINT('Ctrl Pts',(-39.893238251838,27.0262942606764,9.36829843431533));
#11976=CARTESIAN_POINT('Ctrl Pts',(-42.4406501468027,28.2976301604605,9.20951371508965));
#11977=CARTESIAN_POINT('Ctrl Pts',(-42.7538141718088,31.1276146479845,9.05072899586396));
#11978=CARTESIAN_POINT('Ctrl Pts',(-40.5458432066888,32.9252078737001,8.89194427663828));
#11979=CARTESIAN_POINT('Ctrl Pts',(-37.8381936539619,32.0448610117969,8.7331595574126));
#11980=CARTESIAN_POINT('Ctrl Pts',(-37.1096261501333,29.2924579439933,8.57437483818691));
#11981=CARTESIAN_POINT('Ctrl Pts',(-39.0271561460632,27.1878078198326,8.41559011896123));
#11982=CARTESIAN_POINT('Ctrl Pts',(-41.8353046202503,27.6576682343505,8.25680539973555));
#11983=CARTESIAN_POINT('Ctrl Pts',(-42.9632640350674,30.271897164204,8.09802068050986));
#11984=CARTESIAN_POINT('Ctrl Pts',(-41.3784031736155,32.6372074912328,7.93923596128418));
#11985=CARTESIAN_POINT('Ctrl Pts',(-38.5316374790102,32.5881985457519,7.78045124205849));
#11986=CARTESIAN_POINT('Ctrl Pts',(-37.0291331647424,30.1697362755039,7.62166652283281));
#11987=CARTESIAN_POINT('Ctrl Pts',(-38.246408487778,27.5958834047039,7.46288180360713));
#11988=CARTESIAN_POINT('Ctrl Pts',(-41.0690678092901,27.2229594848474,7.30409708438144));
#11989=CARTESIAN_POINT('Ctrl Pts',(-42.9130132431038,29.3923703212235,7.14531236515576));
#11990=CARTESIAN_POINT('Ctrl Pts',(-42.0901431576515,32.1180560714127,6.98652764593008));
#11991=CARTESIAN_POINT('Ctrl Pts',(-39.3537815467508,32.9046964865801,6.8277429267044));
#11992=CARTESIAN_POINT('Ctrl Pts',(-37.209022250832,31.0321352466005,6.66895820747871));
#11993=CARTESIAN_POINT('Ctrl Pts',(-37.6193569815813,28.2146712408483,6.51017348825303));
#11994=CARTESIAN_POINT('Ctrl Pts',(-40.2091310684138,27.0316462206917,6.35138876902734));
#11995=CARTESIAN_POINT('Ctrl Pts',(-42.6074491172863,28.5661000513194,6.19260404980166));
#11996=CARTESIAN_POINT('Ctrl Pts',(-42.618690571971,31.4132655977958,6.03381933057598));
#11997=CARTESIAN_POINT('Ctrl Pts',(-40.2325640667778,32.966609835642,5.8750346113503));
#11998=CARTESIAN_POINT('Ctrl Pts',(-37.6335290001561,31.8040717748601,5.7162498921246));
#11999=CARTESIAN_POINT('Ctrl Pts',(-37.2009590417481,28.9899358060303,5.55746517289893));
#12000=CARTESIAN_POINT('Ctrl Pts',(-39.3308648427259,27.1004969213211,5.39868045367324));
#12001=CARTESIAN_POINT('Ctrl Pts',(-42.0733528266276,27.8655052077231,5.23989573444756));
#12002=CARTESIAN_POINT('Ctrl Pts',(-42.9177205478493,30.58460821633,5.08111101522188));
#12003=CARTESIAN_POINT('Ctrl Pts',(-41.0909633058848,32.7685120601473,4.92232629599619));
#12004=CARTESIAN_POINT('Ctrl Pts',(-38.2654471792087,32.4178888464519,4.76354157677051));
#12005=CARTESIAN_POINT('Ctrl Pts',(-37.0278855065648,29.8537283354108,4.60475685754482));
#12006=CARTESIAN_POINT('Ctrl Pts',(-38.5112455557523,27.4234771169624,4.44597213831914));
#12007=CARTESIAN_POINT('Ctrl Pts',(-41.3575357056293,27.3519900359734,4.28718741909345));
#12008=CARTESIAN_POINT('Ctrl Pts',(-42.9610243424029,29.7047123338834,4.12840269986777));
#12009=CARTESIAN_POINT('Ctrl Pts',(-41.8537441073879,32.3277656126068,3.96961798064209));
#12010=CARTESIAN_POINT('Ctrl Pts',(-39.0493917644644,32.8197879249922,3.81083326141641));
#12011=CARTESIAN_POINT('Ctrl Pts',(-37.1153055577768,30.7303409742253,3.65204854219072));
#12012=CARTESIAN_POINT('Ctrl Pts',(-37.8221094603855,27.9722789230449,3.49326382296504));
#12013=CARTESIAN_POINT('Ctrl Pts',(-40.5227361745428,27.070562027803,3.33447910373935));
#12014=CARTESIAN_POINT('Ctrl Pts',(-42.7448065570598,28.85069719162,3.17569438451367));
#12015=CARTESIAN_POINT('Ctrl Pts',(-42.4540518766068,31.6830001160374,3.01690966528799));
#12016=CARTESIAN_POINT('Ctrl Pts',(-39.9166532459575,32.9745441859394,2.8581249460623));
#12017=CARTESIAN_POINT('Ctrl Pts',(-37.4555571840299,31.5429422906621,2.69934022683662));
#12018=CARTESIAN_POINT('Ctrl Pts',(-37.3238565035427,28.6988020167365,2.54055550761094));
#12019=CARTESIAN_POINT('Ctrl Pts',(-39.6421209553087,27.0458874005518,2.38177078838525));
#12020=CARTESIAN_POINT('Ctrl Pts',(-42.288017822608,28.0974132732372,2.22298606915957));
#12021=CARTESIAN_POINT('Ctrl Pts',(-42.8392720457105,30.8907274554712,2.06420134993389));
#12022=CARTESIAN_POINT('Ctrl Pts',(-40.7912198606381,32.8685921903381,1.9054166307082));
#12023=CARTESIAN_POINT('Ctrl Pts',(-38.0188184697836,32.2203145041505,1.74663191148252));
#12024=CARTESIAN_POINT('Ctrl Pts',(-37.0601570282021,29.5393629015074,1.58784719225684));
#12025=CARTESIAN_POINT('Ctrl Pts',(-38.7928712947239,27.2801422464504,1.42906247303115));
#12026=CARTESIAN_POINT('Ctrl Pts',(-41.6306958817449,27.5108559245266,1.27027775380547));
#12027=CARTESIAN_POINT('Ctrl Pts',(-42.9756374754398,30.0204407538824,1.11149303457979));
#12028=CARTESIAN_POINT('Ctrl Pts',(-41.5964477943764,32.5111109761991,0.952708315354102));
#12029=CARTESIAN_POINT('Ctrl Pts',(-38.7557052213904,32.7033028504944,0.793923596128418));
#12030=CARTESIAN_POINT('Ctrl Pts',(-37.0541564540138,30.4198622099582,0.635138876902736));
#12031=CARTESIAN_POINT('Ctrl Pts',(-38.0493544057376,27.7536501495095,0.47635415767705));
#12032=CARTESIAN_POINT('Ctrl Pts',(-40.8305790077041,27.1407136061552,0.317569438451368));
#12033=CARTESIAN_POINT('Ctrl Pts',(-42.8509979501178,29.1520151888193,0.158784719225683));
#12034=CARTESIAN_POINT('Ctrl Pts',(-42.4575265280738,30.9996488965529,0.0529282397418946));
#12035=CARTESIAN_POINT('Ctrl Pts',(-41.9134659966651,31.635987203375,0.));
#12036=CARTESIAN_POINT('Ctrl Pts',(-41.9134659966651,31.635987203375,0.));
#12037=CARTESIAN_POINT('Ctrl Pts',(-41.9750787519721,31.5780863425442,-1.96186115810562E-16));
#12038=CARTESIAN_POINT('Ctrl Pts',(-42.0333203309463,31.5170349684915,2.22103875014277E-15));
#12039=CARTESIAN_POINT('Ctrl Pts',(-42.0881938461448,31.4532178794343,1.66533453693773E-15));
#12040=CARTESIAN_POINT('Ctrl Pts',(-42.1445200426994,31.38771134338,1.09491901633508E-15));
#12041=CARTESIAN_POINT('Ctrl Pts',(-42.1972979235958,31.3192902871514,-1.47257027708725E-15));
#12042=CARTESIAN_POINT('Ctrl Pts',(-42.246505305796,31.2483223318251,-1.38777878078145E-15));
#12043=CARTESIAN_POINT('Ctrl Pts',(-42.297406955068,31.1749108677304,-1.30006781520595E-15));
#12044=CARTESIAN_POINT('Ctrl Pts',(-42.3444885826855,31.0987735779648,5.02613438679333E-16));
#12045=CARTESIAN_POINT('Ctrl Pts',(-42.3876907051178,31.0202733855454,1.22124532708767E-15));
#12046=CARTESIAN_POINT('Ctrl Pts',(-42.406591633682,30.9859295513619,1.53564677826632E-15));
#12047=CARTESIAN_POINT('Ctrl Pts',(-42.4247495066867,30.9511329365615,1.10529844948776E-15));
#12048=CARTESIAN_POINT('Ctrl Pts',(-42.4421568977288,30.915911843557,1.60982338570648E-15));
#12049=CARTESIAN_POINT('Ctrl Pts',(-42.4516651170732,30.8966734707859,1.88540366920346E-15));
#12050=CARTESIAN_POINT('Ctrl Pts',(-42.460949400319,30.8773084338143,1.31566465613105E-15));
#12051=CARTESIAN_POINT('Ctrl Pts',(-42.4700083335416,30.8578212163121,1.60982338570648E-15));
#12052=CARTESIAN_POINT('Ctrl Pts',(-42.4786583063457,30.8392137382265,1.89070248574673E-15));
#12053=CARTESIAN_POINT('Ctrl Pts',(-42.4871053067842,30.8204888630385,-2.805315957825E-15));
#12054=CARTESIAN_POINT('Ctrl Pts',(-42.4953340038778,30.8016832742127,-2.66453525910038E-15));
#12055=CARTESIAN_POINT('Ctrl Pts',(-42.5318948097226,30.718128432658,-2.0390345590246E-15));
#12056=CARTESIAN_POINT('Ctrl Pts',(-42.5641953969086,30.6328901298495,1.3017395342382E-15));
#12057=CARTESIAN_POINT('Ctrl Pts',(-42.59221149408,30.5463672129356,6.66133814775094E-16));
#12058=CARTESIAN_POINT('Ctrl Pts',(-42.6206898803926,30.4584165952001,2.00400669355727E-17));
#12059=CARTESIAN_POINT('Ctrl Pts',(-42.6447417066998,30.3691378634739,-3.20845694331531E-15));
#12060=CARTESIAN_POINT('Ctrl Pts',(-42.6643023724568,30.2789128079137,-3.3584246494911E-15));
#12061=CARTESIAN_POINT('Ctrl Pts',(-42.6835247634633,30.190248070317,-3.50579887091441E-15));
#12062=CARTESIAN_POINT('Ctrl Pts',(-42.6984102463557,30.1006685472939,-1.83791489597701E-16));
#12063=CARTESIAN_POINT('Ctrl Pts',(-42.7088548140498,30.0105137169402,6.66133814775094E-16));
#12064=CARTESIAN_POINT('Ctrl Pts',(-42.7129849619528,29.9748633392087,1.00222405004665E-15));
#12065=CARTESIAN_POINT('Ctrl Pts',(-42.7164201926426,29.9391228204044,-2.39044314140577E-15));
#12066=CARTESIAN_POINT('Ctrl Pts',(-42.7191520459164,29.9033126170804,-2.52575738102223E-15));
#12067=CARTESIAN_POINT('Ctrl Pts',(-42.720768952831,29.8821175675802,-2.60584606359175E-15));
#12068=CARTESIAN_POINT('Ctrl Pts',(-42.7221394354625,29.8608981026457,-3.21666721681218E-15));
#12069=CARTESIAN_POINT('Ctrl Pts',(-42.723261537278,29.8396584408921,-3.41393580072236E-15));
#12070=CARTESIAN_POINT('Ctrl Pts',(-42.7240084444107,29.8255206374949,-3.54524412795088E-15));
#12071=CARTESIAN_POINT('Ctrl Pts',(-42.724645223022,29.8113738891061,-3.12269885146989E-15));
#12072=CARTESIAN_POINT('Ctrl Pts',(-42.7251709450439,29.7972339960158,-3.08086889333481E-15));
#12073=CARTESIAN_POINT('Ctrl Pts',(-42.7287097000643,29.702055145649,-2.7993018899111E-15));
#12074=CARTESIAN_POINT('Ctrl Pts',(-42.7272297226826,29.6070253269581,6.43470337153603E-17));
#12075=CARTESIAN_POINT('Ctrl Pts',(-42.7206723647361,29.5125432621922,-2.77555756156289E-16));
#12076=CARTESIAN_POINT('Ctrl Pts',(-42.714137496433,29.4183852407328,-6.18285928655555E-16));
#12077=CARTESIAN_POINT('Ctrl Pts',(-42.7025603747006,29.3247702689567,-2.49368351834607E-15));
#12078=CARTESIAN_POINT('Ctrl Pts',(-42.6858349550881,29.2320750778189,-1.77635683940025E-15));
#12079=CARTESIAN_POINT('Ctrl Pts',(-42.6838980906665,29.221340637552,-1.69328780105545E-15));
#12080=CARTESIAN_POINT('Ctrl Pts',(-42.6818921284449,29.2106185215464,-4.13712221908638E-15));
#12081=CARTESIAN_POINT('Ctrl Pts',(-42.6798168585049,29.1999093083932,-4.21884749357559E-15));
#12082=CARTESIAN_POINT('Ctrl Pts',(-42.6622719337603,29.1093705619761,-4.96218911960519E-15));
#12083=CARTESIAN_POINT('Ctrl Pts',(-42.6397776265129,29.019753739261,6.15786555997277E-16));
#12084=CARTESIAN_POINT('Ctrl Pts',(-42.6126092292143,28.9312967674749,6.10622663543836E-16));
#12085=CARTESIAN_POINT('Ctrl Pts',(-42.6018609497875,28.8963016869939,6.08579739980496E-16));
#12086=CARTESIAN_POINT('Ctrl Pts',(-42.5903805354635,28.8614881887874,-1.38856776536099E-15));
#12087=CARTESIAN_POINT('Ctrl Pts',(-42.5781828380702,28.8268713474415,-1.41553435639707E-15));
#12088=CARTESIAN_POINT('Ctrl Pts',(-42.5722285540192,28.8099731985799,-1.42869804932521E-15));
#12089=CARTESIAN_POINT('Ctrl Pts',(-42.5661033314978,28.7931219150712,1.74111828938451E-15));
#12090=CARTESIAN_POINT('Ctrl Pts',(-42.5598087970384,28.776319278537,1.83186799063151E-15));
#12091=CARTESIAN_POINT('Ctrl Pts',(-42.554564129852,28.7623191587432,1.90748152224151E-15));
#12092=CARTESIAN_POINT('Ctrl Pts',(-42.5492048149782,28.7483606199135,-1.45408019805598E-15));
#12093=CARTESIAN_POINT('Ctrl Pts',(-42.5437340670539,28.7344492432458,-1.33226762955019E-15));
#12094=CARTESIAN_POINT('Ctrl Pts',(-42.5095094611057,28.6474206703273,-5.7021695305309E-16));
#12095=CARTESIAN_POINT('Ctrl Pts',(-42.4709064138711,28.5621802195229,1.68864321939785E-15));
#12096=CARTESIAN_POINT('Ctrl Pts',(-42.4282574113239,28.4789597631487,1.4432899320127E-15));
#12097=CARTESIAN_POINT('Ctrl Pts',(-42.3840281853581,28.3926558369106,1.18884585733067E-15));
#12098=CARTESIAN_POINT('Ctrl Pts',(-42.3354475000923,28.3085236412318,1.13314828784959E-16));
#12099=CARTESIAN_POINT('Ctrl Pts',(-42.2828302240828,28.2268253168789,-9.85322934354826E-16));
#12100=CARTESIAN_POINT('Ctrl Pts',(-42.2296353124201,28.1442301033568,-2.09602160961615E-15));
#12101=CARTESIAN_POINT('Ctrl Pts',(-42.1723142774313,28.0641216750719,-2.97253838087967E-16));
#12102=CARTESIAN_POINT('Ctrl Pts',(-42.1111408546837,27.9867862584352,-2.22044604925031E-16));
#12103=CARTESIAN_POINT('Ctrl Pts',(-42.0873237654165,27.9566767036837,-1.92762852498771E-16));
#12104=CARTESIAN_POINT('Ctrl Pts',(-42.062922203311,27.9269877214739,-2.27435711658574E-15));
#12105=CARTESIAN_POINT('Ctrl Pts',(-42.0379504574256,27.897737243879,-2.4980018054066E-15));
#12106=CARTESIAN_POINT('Ctrl Pts',(-42.0179637641745,27.8743259723636,-2.67700081545615E-15));
#12107=CARTESIAN_POINT('Ctrl Pts',(-41.9976117932189,27.8511956157283,-3.20009655856054E-15));
#12108=CARTESIAN_POINT('Ctrl Pts',(-41.9769014344167,27.8283557099806,-3.37230243729891E-15));
#12109=CARTESIAN_POINT('Ctrl Pts',(-41.9653531006681,27.8156199164157,-3.46832641158786E-15));
#12110=CARTESIAN_POINT('Ctrl Pts',(-41.9536984038099,27.8029800953511,7.67357186873025E-16));
#12111=CARTESIAN_POINT('Ctrl Pts',(-41.941943595762,27.7904426685355,6.38378239159465E-16));
#12112=CARTESIAN_POINT('Ctrl Pts',(-41.8728882149596,27.7167896765417,-1.19327910832526E-16));
#12113=CARTESIAN_POINT('Ctrl Pts',(-41.8003322451598,27.6466141188987,5.023733931277E-16));
#12114=CARTESIAN_POINT('Ctrl Pts',(-41.7245876255422,27.5802048475193,6.31439345255558E-16));
#12115=CARTESIAN_POINT('Ctrl Pts',(-41.6603367100057,27.5238727079194,7.40920462602983E-16));
#12116=CARTESIAN_POINT('Ctrl Pts',(-41.5937903710507,27.4702505403911,-6.6592528956053E-16));
#12117=CARTESIAN_POINT('Ctrl Pts',(-41.5251141439217,27.4195295723835,-9.0205620750794E-17));
#12118=CARTESIAN_POINT('Ctrl Pts',(-41.5024248047731,27.4027723145495,1.00001374685776E-16));
#12119=CARTESIAN_POINT('Ctrl Pts',(-41.4795028173951,27.3863318647826,3.04766671757009E-16));
#12120=CARTESIAN_POINT('Ctrl Pts',(-41.4563536803088,27.3702155597188,3.12250225675825E-16));
#12121=CARTESIAN_POINT('Ctrl Pts',(-41.4397590947421,27.3586624982632,3.17614852244211E-16));
#12122=CARTESIAN_POINT('Ctrl Pts',(-41.4230468122245,27.3472754851638,2.16855581531616E-16));
#12123=CARTESIAN_POINT('Ctrl Pts',(-41.4062334184353,27.3360667111883,1.87350135405495E-16));
#12124=CARTESIAN_POINT('Ctrl Pts',(-41.3198795578094,27.2784982679696,3.58096900660736E-17));
#12125=CARTESIAN_POINT('Ctrl Pts',(-41.2307763049236,27.2255680817869,1.44490008086718E-15));
#12126=CARTESIAN_POINT('Ctrl Pts',(-41.1392322045724,27.1775976168508,2.44942954807925E-15));
#12127=CARTESIAN_POINT('Ctrl Pts',(-41.0476881042212,27.1296271519147,3.45395901529133E-15));
#12128=CARTESIAN_POINT('Ctrl Pts',(-40.9537025110736,27.0866154975335,1.9880187375748E-15));
#12129=CARTESIAN_POINT('Ctrl Pts',(-40.8575459263663,27.0489248645033,3.05224595598119E-15));
#12130=CARTESIAN_POINT('Ctrl Pts',(-40.8369779594655,27.0408628093149,3.30417109938035E-15));
#12131=CARTESIAN_POINT('Ctrl Pts',(-40.8163105439644,27.0330443868027,6.92561079676203E-17));
#12132=CARTESIAN_POINT('Ctrl Pts',(-40.7955475841208,27.0254684201926,2.77555756156289E-17));
#12133=CARTESIAN_POINT('Ctrl Pts',(-42.5142224421888,30.0014129136195,9.11258330249199));
#12134=CARTESIAN_POINT('Ctrl Pts',(-42.5159017793566,30.3285506775319,9.09196520028265));
#12135=CARTESIAN_POINT('Ctrl Pts',(-42.4566447890085,30.6551053183166,9.07134709807331));
#12136=CARTESIAN_POINT('Ctrl Pts',(-42.3336250067878,30.9555494376831,9.05072899586397));
#12137=CARTESIAN_POINT('Ctrl Pts',(-42.0178238501021,31.7268123898897,8.99780075612207));
#12138=CARTESIAN_POINT('Ctrl Pts',(-41.2818335283954,32.3260101317949,8.94487251638018));
#12139=CARTESIAN_POINT('Ctrl Pts',(-40.4625634420876,32.4788845257636,8.89194427663829));
#12140=CARTESIAN_POINT('Ctrl Pts',(-39.6432933557798,32.6317589197323,8.83901603689639));
#12141=CARTESIAN_POINT('Ctrl Pts',(-38.7407435048708,32.3383099657646,8.7860877971545));
#12142=CARTESIAN_POINT('Ctrl Pts',(-38.1680406621116,31.7328516441468,8.7331595574126));
#12143=CARTESIAN_POINT('Ctrl Pts',(-37.5953378193524,31.127393322529,8.68023131767071));
#12144=CARTESIAN_POINT('Ctrl Pts',(-37.3524819847428,30.2099256332611,8.62730307792881));
#12145=CARTESIAN_POINT('Ctrl Pts',(-37.5506424000931,29.4004167679338,8.57437483818692));
#12146=CARTESIAN_POINT('Ctrl Pts',(-37.7488028154433,28.5909079026064,8.52144659844502));
#12147=CARTESIAN_POINT('Ctrl Pts',(-38.3879794807532,27.8893578612195,8.46851835870313));
#12148=CARTESIAN_POINT('Ctrl Pts',(-39.1755925591061,27.6168929096124,8.41559011896123));
#12149=CARTESIAN_POINT('Ctrl Pts',(-39.9632056374589,27.3444279580053,8.36266187921934));
#12150=CARTESIAN_POINT('Ctrl Pts',(-40.8992551288546,27.5010480961779,8.30973363947745));
#12151=CARTESIAN_POINT('Ctrl Pts',(-41.5552731103553,28.0150629869065,8.25680539973555));
#12152=CARTESIAN_POINT('Ctrl Pts',(-42.1511257187354,28.4819360331089,8.20873136732103));
#12153=CARTESIAN_POINT('Ctrl Pts',(-42.515956451978,29.2436544912819,8.16065733490651));
#12154=CARTESIAN_POINT('Ctrl Pts',(-42.5208028517601,30.0013273486611,8.11258330249199));
#12155=CARTESIAN_POINT('Origin',(40.,30.,12.2084234471775));
#12156=CARTESIAN_POINT('Ctrl Pts',(36.9237140680981,30.0022179367619,9.70842344717746));
#12157=CARTESIAN_POINT('Ctrl Pts',(36.922516753995,30.1470050693103,9.70090492237387));
#12158=CARTESIAN_POINT('Ctrl Pts',(36.9976393763497,31.3098392937669,9.64045815782839));
#12159=CARTESIAN_POINT('Ctrl Pts',(38.4808972548234,33.3003381457933,9.52708315354102));
#12160=CARTESIAN_POINT('Ctrl Pts',(41.9490301134684,33.0657006782122,9.36829843431533));
#12161=CARTESIAN_POINT('Ctrl Pts',(43.6328194606851,30.0249550147572,9.20951371508965));
#12162=CARTESIAN_POINT('Ctrl Pts',(41.990841947214,26.9611180881373,9.05072899586396));
#12163=CARTESIAN_POINT('Ctrl Pts',(38.5262718341427,26.6794501801396,8.89194427663828));
#12164=CARTESIAN_POINT('Ctrl Pts',(37.0061628405097,28.6614629298378,8.77784242707611));
#12165=CARTESIAN_POINT('Ctrl Pts',(36.9227278999928,29.8387134193989,8.71666881725584));
#12166=CARTESIAN_POINT('Ctrl Pts',(36.9240970871575,29.9975851957844,8.70842344717746));
#12167=CARTESIAN_POINT('Ctrl Pts',(36.9295987310864,29.9965353802945,9.79157655282255));
#12168=CARTESIAN_POINT('Ctrl Pts',(36.9349212372244,30.7003372070082,9.75519455573125));
#12169=CARTESIAN_POINT('Ctrl Pts',(37.5227892072477,32.4385323387372,9.66588431889804));
#12170=CARTESIAN_POINT('Ctrl Pts',(40.4091142878593,33.6090240981732,9.52364584232295));
#12171=CARTESIAN_POINT('Ctrl Pts',(43.2541895529164,31.6147492063695,9.36486112309727));
#12172=CARTESIAN_POINT('Ctrl Pts',(43.1213435063924,28.1406673653848,9.20607640387158));
#12173=CARTESIAN_POINT('Ctrl Pts',(40.1303404706603,26.3695397560852,9.0472916846459));
#12174=CARTESIAN_POINT('Ctrl Pts',(37.424156644603,27.7201137461279,8.90912506762955));
#12175=CARTESIAN_POINT('Ctrl Pts',(36.9337144820332,29.3758544021975,8.8238866903551));
#12176=CARTESIAN_POINT('Ctrl Pts',(36.9305016190507,30.0017249535699,8.79157655282255));
#12177=CARTESIAN_POINT('Ctrl Pts',(41.9134659966651,31.6359872033749,10.));
#12178=CARTESIAN_POINT('Ctrl Pts',(42.4575265280738,30.9996488965529,9.94707176025811));
#12179=CARTESIAN_POINT('Ctrl Pts',(42.8509942844496,29.1520113122851,9.84121528077432));
#12180=CARTESIAN_POINT('Ctrl Pts',(40.8305808300176,27.1407149884891,9.68243056154863));
#12181=CARTESIAN_POINT('Ctrl Pts',(38.0493533010215,27.7536486980057,9.52364584232295));
#12182=CARTESIAN_POINT('Ctrl Pts',(37.0541564147695,30.4198629586065,9.36486112309727));
#12183=CARTESIAN_POINT('Ctrl Pts',(38.7557048443201,32.703302841072,9.20607640387159));
#12184=CARTESIAN_POINT('Ctrl Pts',(41.596448124502,32.5111115852934,9.04729168464589));
#12185=CARTESIAN_POINT('Ctrl Pts',(42.9756378696192,30.0204406213279,8.88850696542022));
#12186=CARTESIAN_POINT('Ctrl Pts',(41.6306961451476,27.5108556326292,8.72972224619452));
#12187=CARTESIAN_POINT('Ctrl Pts',(38.7928711054024,27.2801418020177,8.57093752696886));
#12188=CARTESIAN_POINT('Ctrl Pts',(37.0601565987728,29.5393628566338,8.41215280774316));
#12189=CARTESIAN_POINT('Ctrl Pts',(38.0188181742894,32.220314819778,8.25336808851748));
#12190=CARTESIAN_POINT('Ctrl Pts',(40.7912199788668,32.8685926213582,8.0945833692918));
#12191=CARTESIAN_POINT('Ctrl Pts',(42.8392724649314,30.8907275834786,7.93579865006611));
#12192=CARTESIAN_POINT('Ctrl Pts',(42.2880181612085,28.0974129938986,7.77701393084043));
#12193=CARTESIAN_POINT('Ctrl Pts',(39.6421209022521,27.0458869626938,7.61822921161475));
#12194=CARTESIAN_POINT('Ctrl Pts',(37.3238561079106,28.698801824901,7.45944449238905));
#12195=CARTESIAN_POINT('Ctrl Pts',(37.4555568077712,31.5429425185067,7.30065977316339));
#12196=CARTESIAN_POINT('Ctrl Pts',(39.9166532336493,32.9745446259184,7.14187505393769));
#12197=CARTESIAN_POINT('Ctrl Pts',(42.45405223946,31.6830003648061,6.98309033471202));
#12198=CARTESIAN_POINT('Ctrl Pts',(42.7448069629157,28.8506970217256,6.82430561548633));
#12199=CARTESIAN_POINT('Ctrl Pts',(40.5227362518339,27.0705615946279,6.66552089626065));
#12200=CARTESIAN_POINT('Ctrl Pts',(37.8221091383592,27.9722786232342,6.50673617703496));
#12201=CARTESIAN_POINT('Ctrl Pts',(37.11530513124,30.7303410822086,6.34795145780927));
#12202=CARTESIAN_POINT('Ctrl Pts',(39.0493916239058,32.8197883419346,6.18916673858359));
#12203=CARTESIAN_POINT('Ctrl Pts',(41.8537443814859,32.3277659567929,6.03038201935791));
#12204=CARTESIAN_POINT('Ctrl Pts',(42.9610247802256,29.7047122902225,5.87159730013223));
#12205=CARTESIAN_POINT('Ctrl Pts',(41.3575359063571,27.3519896444331,5.71281258090654));
#12206=CARTESIAN_POINT('Ctrl Pts',(38.5112453356222,27.423476735993,5.55402786168086));
#12207=CARTESIAN_POINT('Ctrl Pts',(37.0278850671023,29.8537283137827,5.39524314245517));
#12208=CARTESIAN_POINT('Ctrl Pts',(38.2654469227344,32.4178892039655,5.2364584232295));
#12209=CARTESIAN_POINT('Ctrl Pts',(41.0909634671967,32.7685124695048,5.07767370400381));
#12210=CARTESIAN_POINT('Ctrl Pts',(42.9177209792689,30.5846083027713,4.91888898477813));
#12211=CARTESIAN_POINT('Ctrl Pts',(42.0733531331975,27.8655048921126,4.76010426555244));
#12212=CARTESIAN_POINT('Ctrl Pts',(39.3308647437863,27.1004964925952,4.60131954632676));
#12213=CARTESIAN_POINT('Ctrl Pts',(37.2009586278766,28.9899356566802,4.44253482710108));
#12214=CARTESIAN_POINT('Ctrl Pts',(37.6335286502452,31.8040720416137,4.28375010787539));
#12215=CARTESIAN_POINT('Ctrl Pts',(40.232564101165,32.9666102742903,4.12496538864971));
#12216=CARTESIAN_POINT('Ctrl Pts',(42.6186909591757,31.4132658067643,3.96618066942402));
#12217=CARTESIAN_POINT('Ctrl Pts',(42.6074495028282,28.5660998392996,3.80739595019834));
#12218=CARTESIAN_POINT('Ctrl Pts',(40.2091310993371,27.0316457817867,3.64861123097266));
#12219=CARTESIAN_POINT('Ctrl Pts',(37.6193566295732,28.2146709768635,3.48982651174698));
#12220=CARTESIAN_POINT('Ctrl Pts',(37.209021838156,31.0321353992193,3.33104179252129));
#12221=CARTESIAN_POINT('Ctrl Pts',(39.3537814511937,32.9046969160638,3.17225707329561));
#12222=CARTESIAN_POINT('Ctrl Pts',(42.0901434667156,32.1180563846122,3.01347235406992));
#12223=CARTESIAN_POINT('Ctrl Pts',(42.9130136738057,29.3923702313403,2.85468763484424));
#12224=CARTESIAN_POINT('Ctrl Pts',(41.0690679674053,27.2229590743015,2.69590291561856));
#12225=CARTESIAN_POINT('Ctrl Pts',(38.2464082284125,27.5958830490882,2.53711819639287));
#12226=CARTESIAN_POINT('Ctrl Pts',(37.0291327256062,30.1697363008652,2.37833347716719));
#12227=CARTESIAN_POINT('Ctrl Pts',(38.5316372616326,32.5881989279464,2.2195487579415));
#12228=CARTESIAN_POINT('Ctrl Pts',(41.3784033779123,32.6372078821259,2.06076403871582));
#12229=CARTESIAN_POINT('Ctrl Pts',(42.9632644723377,30.2718972026101,1.90197931949014));
#12230=CARTESIAN_POINT('Ctrl Pts',(41.8353048932223,27.6576678913952,1.74319460026445));
#12231=CARTESIAN_POINT('Ctrl Pts',(39.0271559993481,27.1878073976584,1.58440988103877));
#12232=CARTESIAN_POINT('Ctrl Pts',(37.1096257278314,29.2924578512643,1.42562516181309));
#12233=CARTESIAN_POINT('Ctrl Pts',(37.8381933254868,32.0448612920238,1.26684044258741));
#12234=CARTESIAN_POINT('Ctrl Pts',(40.5458433024136,32.9252083471976,1.10805572336172));
#12235=CARTESIAN_POINT('Ctrl Pts',(42.7538145542223,31.1276147393353,0.949271004136036));
#12236=CARTESIAN_POINT('Ctrl Pts',(42.4406505467311,28.2976300464195,0.790486284910354));
#12237=CARTESIAN_POINT('Ctrl Pts',(39.8932381788789,27.0262935717237,0.631701565684669));
#12238=CARTESIAN_POINT('Ctrl Pts',(37.4433110051919,28.4770232868416,0.472916846458986));
#12239=CARTESIAN_POINT('Ctrl Pts',(37.3344967579085,31.3226381965804,0.314132127233303));
#12240=CARTESIAN_POINT('Ctrl Pts',(39.6648948723936,32.9561497373541,0.155347408007618));
#12241=CARTESIAN_POINT('Ctrl Pts',(42.3041009889826,31.8858668894737,-0.00343731121806406));
#12242=CARTESIAN_POINT('Ctrl Pts',(42.8298459315877,29.0839076313313,-0.162222030443749));
#12243=CARTESIAN_POINT('Ctrl Pts',(41.4590097705807,27.7841423687619,-0.268078509927538));
#12244=CARTESIAN_POINT('Ctrl Pts',(40.6501999979751,27.5679131979649,-0.321006749669432));
#12245=CARTESIAN_POINT('Ctrl Pts',(42.0543315503421,31.7564253212268,10.1070022498898));
#12246=CARTESIAN_POINT('Ctrl Pts',(42.6384447339141,31.0732410562991,10.0540740101479));
#12247=CARTESIAN_POINT('Ctrl Pts',(43.0608788024441,29.0895840748975,9.94821753066413));
#12248=CARTESIAN_POINT('Ctrl Pts',(40.8917265356104,26.9302201236894,9.78943281143845));
#12249=CARTESIAN_POINT('Ctrl Pts',(37.9057505781308,27.5882767914968,9.63064809221276));
#12250=CARTESIAN_POINT('Ctrl Pts',(36.8372892802593,30.4507724329508,9.47186337298707));
#12251=CARTESIAN_POINT('Ctrl Pts',(38.6641023144879,32.9023146093124,9.3130786537614));
#12252=CARTESIAN_POINT('Ctrl Pts',(41.7139754541574,32.6959746162664,9.1542939345357));
#12253=CARTESIAN_POINT('Ctrl Pts',(43.1946983999746,30.0219454191376,8.99550921531004));
#12254=CARTESIAN_POINT('Ctrl Pts',(41.7507447458364,27.3276097844653,8.83672449608433));
#12255=CARTESIAN_POINT('Ctrl Pts',(38.7040046816492,27.0799112613917,8.67793977685867));
#12256=CARTESIAN_POINT('Ctrl Pts',(36.8437311858523,29.5054516680589,8.51915505763297));
#12257=CARTESIAN_POINT('Ctrl Pts',(37.8729675162166,32.3837699723495,8.3603703384073));
#12258=CARTESIAN_POINT('Ctrl Pts',(40.849468017033,33.0797726938475,8.2015856191816));
#12259=CARTESIAN_POINT('Ctrl Pts',(43.0482940459313,30.9563011732056,8.04280089995593));
#12260=CARTESIAN_POINT('Ctrl Pts',(42.4564574988625,27.9573483298281,7.88401618073024));
#12261=CARTESIAN_POINT('Ctrl Pts',(39.6157745562278,26.8284110476005,7.72523146150455));
#12262=CARTESIAN_POINT('Ctrl Pts',(37.1268437273741,28.6030102081707,7.56644674227888));
#12263=CARTESIAN_POINT('Ctrl Pts',(37.2682399703162,31.6565308720704,7.40766202305319));
#12264=CARTESIAN_POINT('Ctrl Pts',(39.9105174107972,33.193524673851,7.24887730382751));
#12265=CARTESIAN_POINT('Ctrl Pts',(42.6347146750959,31.8068994979186,7.09009258460182));
#12266=CARTESIAN_POINT('Ctrl Pts',(42.9468741819003,28.7660876267013,6.93130786537614));
#12267=CARTESIAN_POINT('Ctrl Pts',(40.5612190530281,26.854902176768,6.77252314615045));
#12268=CARTESIAN_POINT('Ctrl Pts',(37.6617771530468,27.8230018161528,6.61373842692477));
#12269=CARTESIAN_POINT('Ctrl Pts',(36.9029396433842,30.7841073373173,6.45495370769908));
#12270=CARTESIAN_POINT('Ctrl Pts',(38.9794097295519,33.0273755406259,6.29616898847341));
#12271=CARTESIAN_POINT('Ctrl Pts',(41.9902133488618,32.4991314479517,6.13738426924772));
#12272=CARTESIAN_POINT('Ctrl Pts',(43.1790095240595,29.6829737974538,5.97859955002203));
#12273=CARTESIAN_POINT('Ctrl Pts',(41.4574749945973,27.1570483987933,5.81981483079636));
#12274=CARTESIAN_POINT('Ctrl Pts',(38.4016461838984,27.2337982275802,5.66103011157067));
#12275=CARTESIAN_POINT('Ctrl Pts',(36.8090838883282,29.8429600837215,5.50224539234499));
#12276=CARTESIAN_POINT('Ctrl Pts',(38.1377525816606,32.595889388991,5.3434606731193));
#12277=CARTESIAN_POINT('Ctrl Pts',(41.1712780236696,32.972324840646,5.18467595389362));
#12278=CARTESIAN_POINT('Ctrl Pts',(43.1325177835687,30.6276460010621,5.02589123466794));
#12279=CARTESIAN_POINT('Ctrl Pts',(42.2259892592561,27.708367615716,4.86710651544225));
#12280=CARTESIAN_POINT('Ctrl Pts',(39.2816043396215,26.8870408222718,4.70832179621657));
#12281=CARTESIAN_POINT('Ctrl Pts',(36.9948987797599,28.915576732498,4.54953707699089));
#12282=CARTESIAN_POINT('Ctrl Pts',(37.4593137451855,31.9368842303111,4.3907523577652));
#12283=CARTESIAN_POINT('Ctrl Pts',(40.2496850068582,33.1850062110669,4.23196763853952));
#12284=CARTESIAN_POINT('Ctrl Pts',(42.8114737692787,31.5173076192186,4.07318291931383));
#12285=CARTESIAN_POINT('Ctrl Pts',(42.7994047393158,28.4605389668269,3.91439820008815));
#12286=CARTESIAN_POINT('Ctrl Pts',(40.2245269141311,26.8131214593336,3.75561348086246));
#12287=CARTESIAN_POINT('Ctrl Pts',(37.4440984085924,28.0832386118368,3.59682876163679));
#12288=CARTESIAN_POINT('Ctrl Pts',(37.0035555875124,31.1081191505555,3.4380440424111));
#12289=CARTESIAN_POINT('Ctrl Pts',(39.3062081293617,33.1185349147835,3.27925932318542));
#12290=CARTESIAN_POINT('Ctrl Pts',(42.2440156636693,32.2739834749591,3.12047460395973));
#12291=CARTESIAN_POINT('Ctrl Pts',(43.1274639356577,29.3476377386061,2.96168988473405));
#12292=CARTESIAN_POINT('Ctrl Pts',(41.147770620815,27.01851885521,2.80290516550837));
#12293=CARTESIAN_POINT('Ctrl Pts',(38.1173122966015,27.4188967498883,2.64412044628268));
#12294=CARTESIAN_POINT('Ctrl Pts',(36.810423396965,30.1822319490984,2.485335727057));
#12295=CARTESIAN_POINT('Ctrl Pts',(38.4235393228663,32.7787369754722,2.32655100783132));
#12296=CARTESIAN_POINT('Ctrl Pts',(41.4798786878256,32.8313538711974,2.16776628860563));
#12297=CARTESIAN_POINT('Ctrl Pts',(43.1814140978417,30.2919137328519,2.00898156937995));
#12298=CARTESIAN_POINT('Ctrl Pts',(41.970416382217,27.4852300691662,1.85019685015426));
#12299=CARTESIAN_POINT('Ctrl Pts',(38.9555371626234,26.9807793821798,1.69141213092858));
#12300=CARTESIAN_POINT('Ctrl Pts',(36.8968421336142,29.2403700082061,1.5326274117029));
#12301=CARTESIAN_POINT('Ctrl Pts',(37.6790454259794,32.1953999055115,1.37384269247722));
#12302=CARTESIAN_POINT('Ctrl Pts',(40.5860271986257,33.1405563566039,1.21505797325153));
#12303=CARTESIAN_POINT('Ctrl Pts',(42.9565448941293,31.2106274894275,1.05627325402585));
#12304=CARTESIAN_POINT('Ctrl Pts',(42.620326376454,28.1723049627795,0.897488534800165));
#12305=CARTESIAN_POINT('Ctrl Pts',(39.8853785863542,26.8073752302313,0.73870381557448));
#12306=CARTESIAN_POINT('Ctrl Pts',(37.2550926561533,28.3649047760814,0.579919096348797));
#12307=CARTESIAN_POINT('Ctrl Pts',(37.1382677208211,31.4200081849681,0.421134377123114));
#12308=CARTESIAN_POINT('Ctrl Pts',(39.6402251006691,33.1737755902464,0.262349657897428));
#12309=CARTESIAN_POINT('Ctrl Pts',(42.4737243123688,32.0247006518765,0.103564938671747));
#12310=CARTESIAN_POINT('Ctrl Pts',(43.0381735499873,29.0164667366633,-0.0552197805539385));
#12311=CARTESIAN_POINT('Ctrl Pts',(41.5664191624963,27.6210153455288,-0.161076260037727));
#12312=CARTESIAN_POINT('Ctrl Pts',(40.698066426161,27.3888678140614,-0.214004499779622));
#12313=CARTESIAN_POINT('Ctrl Pts',(42.1951971040191,31.8768634390787,10.2140044997796));
#12314=CARTESIAN_POINT('Ctrl Pts',(42.8193629397544,31.1468332160454,10.1610762600377));
#12315=CARTESIAN_POINT('Ctrl Pts',(43.2707633204387,29.02715683751,10.0552197805539));
#12316=CARTESIAN_POINT('Ctrl Pts',(40.9528722412032,26.7197252588896,9.89643506132826));
#12317=CARTESIAN_POINT('Ctrl Pts',(37.7621478552401,27.4229048849878,9.73765034210257));
#12318=CARTESIAN_POINT('Ctrl Pts',(36.6204221457491,30.4816819072951,9.57886562287689));
#12319=CARTESIAN_POINT('Ctrl Pts',(38.5724997846557,33.1013263775528,9.4200809036512));
#12320=CARTESIAN_POINT('Ctrl Pts',(41.8315027838129,32.8808376472393,9.26129618442552));
#12321=CARTESIAN_POINT('Ctrl Pts',(43.4137589303298,30.0234502169474,9.10251146519984));
#12322=CARTESIAN_POINT('Ctrl Pts',(41.8707933465252,27.1443639363013,8.94372674597414));
#12323=CARTESIAN_POINT('Ctrl Pts',(38.6151382578959,26.8796807207656,8.78494202674849));
#12324=CARTESIAN_POINT('Ctrl Pts',(36.6273057729317,29.4715404794841,8.62615730752277));
#12325=CARTESIAN_POINT('Ctrl Pts',(37.7271168581437,32.547225124921,8.46737258829711));
#12326=CARTESIAN_POINT('Ctrl Pts',(40.9077160551992,33.2909527663368,8.30858786907142));
#12327=CARTESIAN_POINT('Ctrl Pts',(43.2573156269313,31.0218747629328,8.14980314984574));
#12328=CARTESIAN_POINT('Ctrl Pts',(42.6248968365165,27.8172836657576,7.99101843062005));
#12329=CARTESIAN_POINT('Ctrl Pts',(39.5894282102036,26.6109351325072,7.83223371139437));
#12330=CARTESIAN_POINT('Ctrl Pts',(36.9298313468376,28.5072185914405,7.67344899216868));
#12331=CARTESIAN_POINT('Ctrl Pts',(37.0809231328611,31.7701192256341,7.514664272943));
#12332=CARTESIAN_POINT('Ctrl Pts',(39.904381587945,33.4125047217835,7.35587955371733));
#12333=CARTESIAN_POINT('Ctrl Pts',(42.8153771107317,31.9307986310311,7.19709483449163));
#12334=CARTESIAN_POINT('Ctrl Pts',(43.1489414008849,28.681478231677,7.03831011526596));
#12335=CARTESIAN_POINT('Ctrl Pts',(40.5997018542224,26.6392427589081,6.87952539604026));
#12336=CARTESIAN_POINT('Ctrl Pts',(37.5014451677344,27.6737250090714,6.72074067681458));
#12337=CARTESIAN_POINT('Ctrl Pts',(36.6905741555285,30.8378735924259,6.5619559575889));
#12338=CARTESIAN_POINT('Ctrl Pts',(38.9094278351979,33.2349627393171,6.40317123836321));
#12339=CARTESIAN_POINT('Ctrl Pts',(42.1266823162377,32.6704969391105,6.24438651913754));
#12340=CARTESIAN_POINT('Ctrl Pts',(43.3969942678934,29.6612353046849,6.08560179991184));
#12341=CARTESIAN_POINT('Ctrl Pts',(41.5574140828376,26.9621071531534,5.92681708068618));
#12342=CARTESIAN_POINT('Ctrl Pts',(38.2920470321746,27.0441197191674,5.76803236146047));
#12343=CARTESIAN_POINT('Ctrl Pts',(36.5902827095542,29.8321918536604,5.60924764223481));
#12344=CARTESIAN_POINT('Ctrl Pts',(38.0100582405868,32.7738895740165,5.45046292300911));
#12345=CARTESIAN_POINT('Ctrl Pts',(41.2515925801425,33.1761372117873,5.29167820378343));
#12346=CARTESIAN_POINT('Ctrl Pts',(43.3473145878683,30.6706836993528,5.13289348455775));
#12347=CARTESIAN_POINT('Ctrl Pts',(42.3786253853148,27.5512303393194,4.97410876533207));
#12348=CARTESIAN_POINT('Ctrl Pts',(39.2323439354566,26.6735851519484,4.81532404610638));
#12349=CARTESIAN_POINT('Ctrl Pts',(36.7888389316434,28.8412178083158,4.6565393268807));
#12350=CARTESIAN_POINT('Ctrl Pts',(37.2850988401258,32.0696964190085,4.49775460765501));
#12351=CARTESIAN_POINT('Ctrl Pts',(40.2668059125513,33.4034021478436,4.33896988842933));
#12352=CARTESIAN_POINT('Ctrl Pts',(43.0042565793815,31.6213494316729,4.18018516920364));
#12353=CARTESIAN_POINT('Ctrl Pts',(42.9913599758034,28.3549780943543,4.02140044997796));
#12354=CARTESIAN_POINT('Ctrl Pts',(40.2399227289251,26.5945971368806,3.86261573075228));
#12355=CARTESIAN_POINT('Ctrl Pts',(37.2688401876116,27.9518062468101,3.7038310115266));
#12356=CARTESIAN_POINT('Ctrl Pts',(36.7980893368689,31.1841029018916,3.54504629230091));
#12357=CARTESIAN_POINT('Ctrl Pts',(39.2586348075297,33.3323729135034,3.38626157307523));
#12358=CARTESIAN_POINT('Ctrl Pts',(42.3978878606232,32.4299105653059,3.22747685384954));
#12359=CARTESIAN_POINT('Ctrl Pts',(43.3419141975094,29.302905245872,3.06869213462386));
#12360=CARTESIAN_POINT('Ctrl Pts',(41.2264732742248,26.8140786361186,2.90990741539818));
#12361=CARTESIAN_POINT('Ctrl Pts',(37.9882163647905,27.2419104506884,2.75112269617249));
#12362=CARTESIAN_POINT('Ctrl Pts',(36.5917140683237,30.1947275973316,2.59233797694681));
#12363=CARTESIAN_POINT('Ctrl Pts',(38.3154413841,32.9692750229979,2.43355325772113));
#12364=CARTESIAN_POINT('Ctrl Pts',(41.5813539977387,33.0254998602688,2.27476853849544));
#12365=CARTESIAN_POINT('Ctrl Pts',(43.3995637233459,30.3119302630937,2.11598381926976));
#12366=CARTESIAN_POINT('Ctrl Pts',(42.1055278712115,27.3127922469373,1.95719910004408));
#12367=CARTESIAN_POINT('Ctrl Pts',(38.8839183258989,26.7737513667013,1.79841438081839));
#12368=CARTESIAN_POINT('Ctrl Pts',(36.6840585393969,29.1882821651479,1.63962966159271));
#12369=CARTESIAN_POINT('Ctrl Pts',(37.519897526472,32.3459385189991,1.48084494236703));
#12370=CARTESIAN_POINT('Ctrl Pts',(40.6262110948378,33.3559043660104,1.32206022314134));
#12371=CARTESIAN_POINT('Ctrl Pts',(43.1592752340363,31.2936402395195,1.16327550391566));
#12372=CARTESIAN_POINT('Ctrl Pts',(42.8000022061769,28.0469798791396,1.00449078468998));
#12373=CARTESIAN_POINT('Ctrl Pts',(39.8775189938294,26.5884568887389,0.84570606546429));
#12374=CARTESIAN_POINT('Ctrl Pts',(37.0668743071149,28.2527862653212,0.686921346238607));
#12375=CARTESIAN_POINT('Ctrl Pts',(36.9420386837336,31.5173781733559,0.528136627012925));
#12376=CARTESIAN_POINT('Ctrl Pts',(39.6155553289446,33.3914014431387,0.369351907787239));
#12377=CARTESIAN_POINT('Ctrl Pts',(42.643347635755,32.1635344142794,0.210567188561557));
#12378=CARTESIAN_POINT('Ctrl Pts',(43.2465011683868,28.9490258419954,0.0517824693358725));
#12379=CARTESIAN_POINT('Ctrl Pts',(41.6738285544119,27.4578883222956,-0.0540740101479163));
#12380=CARTESIAN_POINT('Ctrl Pts',(40.7459328543469,27.2098224301578,-0.107002249889811));
#12381=CARTESIAN_POINT('Ctrl Pts',(42.3360626576962,31.9973015569306,10.3210067496694));
#12382=CARTESIAN_POINT('Ctrl Pts',(43.0002811455947,31.2204253757916,10.2680785099275));
#12383=CARTESIAN_POINT('Ctrl Pts',(43.4806478384333,28.9647296001224,10.1622220304437));
#12384=CARTESIAN_POINT('Ctrl Pts',(41.0140179467961,26.5092303940899,10.0034373112181));
#12385=CARTESIAN_POINT('Ctrl Pts',(37.6185451323494,27.2575329784789,9.84465259199238));
#12386=CARTESIAN_POINT('Ctrl Pts',(36.4035550112389,30.5125913816394,9.6858678727667));
#12387=CARTESIAN_POINT('Ctrl Pts',(38.4808972548234,33.3003381457933,9.52708315354102));
#12388=CARTESIAN_POINT('Ctrl Pts',(41.9490301134684,33.0657006782122,9.36829843431533));
#12389=CARTESIAN_POINT('Ctrl Pts',(43.6328194606851,30.0249550147572,9.20951371508965));
#12390=CARTESIAN_POINT('Ctrl Pts',(41.990841947214,26.9611180881373,9.05072899586396));
#12391=CARTESIAN_POINT('Ctrl Pts',(38.5262718341427,26.6794501801396,8.89194427663828));
#12392=CARTESIAN_POINT('Ctrl Pts',(36.4108803600112,29.4376292909092,8.73315955741259));
#12393=CARTESIAN_POINT('Ctrl Pts',(37.5812662000709,32.7106802774926,8.57437483818692));
#12394=CARTESIAN_POINT('Ctrl Pts',(40.9659640933653,33.5021328388261,8.41559011896122));
#12395=CARTESIAN_POINT('Ctrl Pts',(43.4663372079312,31.0874483526599,8.25680539973555));
#12396=CARTESIAN_POINT('Ctrl Pts',(42.7933361741705,27.6772190016871,8.09802068050986));
#12397=CARTESIAN_POINT('Ctrl Pts',(39.5630818641794,26.3934592174139,7.93923596128418));
#12398=CARTESIAN_POINT('Ctrl Pts',(36.7328189663011,28.4114269747102,7.78045124205849));
#12399=CARTESIAN_POINT('Ctrl Pts',(36.8936062954061,31.8837075791978,7.62166652283282));
#12400=CARTESIAN_POINT('Ctrl Pts',(39.8982457650928,33.6314847697161,7.46288180360713));
#12401=CARTESIAN_POINT('Ctrl Pts',(42.9960395463676,32.0546977641436,7.30409708438144));
#12402=CARTESIAN_POINT('Ctrl Pts',(43.3510086198694,28.5968688366528,7.14531236515576));
#12403=CARTESIAN_POINT('Ctrl Pts',(40.6381846554167,26.4235833410482,6.98652764593007));
#12404=CARTESIAN_POINT('Ctrl Pts',(37.3411131824219,27.5244482019901,6.8277429267044));
#12405=CARTESIAN_POINT('Ctrl Pts',(36.4782086676728,30.8916398475345,6.66895820747871));
#12406=CARTESIAN_POINT('Ctrl Pts',(38.8394459408439,33.4425499380084,6.51017348825303));
#12407=CARTESIAN_POINT('Ctrl Pts',(42.2631512836135,32.8418624302693,6.35138876902734));
#12408=CARTESIAN_POINT('Ctrl Pts',(43.6149790117272,29.6394968119162,6.19260404980166));
#12409=CARTESIAN_POINT('Ctrl Pts',(41.657353171078,26.7671659075135,6.03381933057598));
#12410=CARTESIAN_POINT('Ctrl Pts',(38.1824478804507,26.8544412107546,5.87503461135029));
#12411=CARTESIAN_POINT('Ctrl Pts',(36.3714815307802,29.8214236235992,5.71624989212461));
#12412=CARTESIAN_POINT('Ctrl Pts',(37.882363899513,32.951889759042,5.55746517289893));
#12413=CARTESIAN_POINT('Ctrl Pts',(41.3319071366153,33.3799495829286,5.39868045367324));
#12414=CARTESIAN_POINT('Ctrl Pts',(43.562111392168,30.7137213976436,5.23989573444756));
#12415=CARTESIAN_POINT('Ctrl Pts',(42.5312615113734,27.3940930629228,5.08111101522188));
#12416=CARTESIAN_POINT('Ctrl Pts',(39.1830835312918,26.4601294816251,4.92232629599619));
#12417=CARTESIAN_POINT('Ctrl Pts',(36.5827790835267,28.7668588841336,4.7635415767705));
#12418=CARTESIAN_POINT('Ctrl Pts',(37.1108839350661,32.202508607706,4.60475685754482));
#12419=CARTESIAN_POINT('Ctrl Pts',(40.2839268182445,33.6217980846202,4.44597213831914));
#12420=CARTESIAN_POINT('Ctrl Pts',(43.1970393894843,31.7253912441272,4.28718741909346));
#12421=CARTESIAN_POINT('Ctrl Pts',(43.1833152122909,28.2494172218816,4.12840269986777));
#12422=CARTESIAN_POINT('Ctrl Pts',(40.255318543719,26.3760728144276,3.96961798064209));
#12423=CARTESIAN_POINT('Ctrl Pts',(37.0935819666309,27.8203738817834,3.8108332614164));
#12424=CARTESIAN_POINT('Ctrl Pts',(36.5926230862254,31.2600866532277,3.65204854219072));
#12425=CARTESIAN_POINT('Ctrl Pts',(39.2110614856976,33.5462109122232,3.49326382296504));
#12426=CARTESIAN_POINT('Ctrl Pts',(42.551760057577,32.5858376556528,3.33447910373935));
#12427=CARTESIAN_POINT('Ctrl Pts',(43.5563644593613,29.2581727531378,3.17569438451367));
#12428=CARTESIAN_POINT('Ctrl Pts',(41.3051759276346,26.6096384170271,3.01690966528799));
#12429=CARTESIAN_POINT('Ctrl Pts',(37.8591204329795,27.0649241514885,2.85812494606231));
#12430=CARTESIAN_POINT('Ctrl Pts',(36.3730047396825,30.2072232455647,2.69934022683662));
#12431=CARTESIAN_POINT('Ctrl Pts',(38.2073434453337,33.1598130705237,2.54055550761094));
#12432=CARTESIAN_POINT('Ctrl Pts',(41.6828293076519,33.2196458493402,2.38177078838525));
#12433=CARTESIAN_POINT('Ctrl Pts',(43.6177133488499,30.3319467933355,2.22298606915957));
#12434=CARTESIAN_POINT('Ctrl Pts',(42.2406393602062,27.1403544247083,2.06420134993389));
#12435=CARTESIAN_POINT('Ctrl Pts',(38.8122994891743,26.5667233512227,1.9054166307082));
#12436=CARTESIAN_POINT('Ctrl Pts',(36.4712749451797,29.1361943220897,1.74663191148252));
#12437=CARTESIAN_POINT('Ctrl Pts',(37.3607496269647,32.4964771324867,1.58784719225684));
#12438=CARTESIAN_POINT('Ctrl Pts',(40.6663949910499,33.5712523754168,1.42906247303115));
#12439=CARTESIAN_POINT('Ctrl Pts',(43.3620055739433,31.3766529896116,1.27027775380547));
#12440=CARTESIAN_POINT('Ctrl Pts',(42.9796780358998,27.9216547954996,1.11149303457979));
#12441=CARTESIAN_POINT('Ctrl Pts',(39.8696594013047,26.3695385472464,0.952708315354102));
#12442=CARTESIAN_POINT('Ctrl Pts',(36.8786559580763,28.1406677545611,0.793923596128418));
#12443=CARTESIAN_POINT('Ctrl Pts',(36.7458096466462,31.6147481617437,0.635138876902736));
#12444=CARTESIAN_POINT('Ctrl Pts',(39.5908855572201,33.609027296031,0.47635415767705));
#12445=CARTESIAN_POINT('Ctrl Pts',(42.8129709591412,32.3023681766822,0.317569438451369));
#12446=CARTESIAN_POINT('Ctrl Pts',(43.4548287867864,28.8815849473274,0.158784719225683));
#12447=CARTESIAN_POINT('Ctrl Pts',(41.7812379463276,27.2947612990625,0.0529282397418946));
#12448=CARTESIAN_POINT('Ctrl Pts',(40.7937992825328,27.0307770462543,0.));
#12449=CARTESIAN_POINT('Ctrl Pts',(40.7937992825328,27.0307770462543,0.));
#12450=CARTESIAN_POINT('Ctrl Pts',(40.8868532983231,27.0648166209,1.23206627813231E-16));
#12451=CARTESIAN_POINT('Ctrl Pts',(40.9778400910404,27.1036256541919,2.12059168736638E-15));
#12452=CARTESIAN_POINT('Ctrl Pts',(41.066551880518,27.1468754141207,1.88737914186277E-15));
#12453=CARTESIAN_POINT('Ctrl Pts',(41.1572334993246,27.1910855271895,1.64898815373364E-15));
#12454=CARTESIAN_POINT('Ctrl Pts',(41.2455386280921,27.239936384657,1.66196107955855E-15));
#12455=CARTESIAN_POINT('Ctrl Pts',(41.3312163993864,27.293122419604,1.66533453693773E-15));
#12456=CARTESIAN_POINT('Ctrl Pts',(41.4141658054003,27.3446147721763,1.6686005682734E-15));
#12457=CARTESIAN_POINT('Ctrl Pts',(41.4946528486676,27.4001714580703,-1.01232175488034E-15));
#12458=CARTESIAN_POINT('Ctrl Pts',(41.5724161625969,27.4595458715911,-7.21644966006352E-16));
#12459=CARTESIAN_POINT('Ctrl Pts',(41.640459062285,27.5114984834218,-4.67302775741614E-16));
#12460=CARTESIAN_POINT('Ctrl Pts',(41.7064163099332,27.5663747599262,-2.34369271321042E-15));
#12461=CARTESIAN_POINT('Ctrl Pts',(41.7700875460549,27.6240224703129,-3.10862446895044E-15));
#12462=CARTESIAN_POINT('Ctrl Pts',(41.7834301864647,27.6361028494133,-3.26891991751667E-15));
#12463=CARTESIAN_POINT('Ctrl Pts',(41.7966742105369,27.6483068338884,-2.63665242192149E-17));
#12464=CARTESIAN_POINT('Ctrl Pts',(41.8098005949636,27.6606167186647,-5.55111512312578E-17));
#12465=CARTESIAN_POINT('Ctrl Pts',(41.8822281775529,27.7285390929699,-2.1632275108547E-16));
#12466=CARTESIAN_POINT('Ctrl Pts',(41.9511900419254,27.799782684138,-1.11617369221794E-15));
#12467=CARTESIAN_POINT('Ctrl Pts',(42.016446845218,27.8740563163129,-1.02695629777827E-15));
#12468=CARTESIAN_POINT('Ctrl Pts',(42.0813423298977,27.9479187048411,-9.38232888694729E-16));
#12469=CARTESIAN_POINT('Ctrl Pts',(42.1425741539473,28.0247784714532,-1.19599204607943E-15));
#12470=CARTESIAN_POINT('Ctrl Pts',(42.1998633142192,28.1043759954772,-9.71445146547012E-16));
#12471=CARTESIAN_POINT('Ctrl Pts',(42.2557183977693,28.1819810141868,-7.52519161686897E-16));
#12472=CARTESIAN_POINT('Ctrl Pts',(42.3078260044473,28.2621891813364,1.94691714197589E-15));
#12473=CARTESIAN_POINT('Ctrl Pts',(42.3558807009596,28.3447740093935,2.58126853225349E-15));
#12474=CARTESIAN_POINT('Ctrl Pts',(42.3766082864569,28.3803955866496,2.85488534042471E-15));
#12475=CARTESIAN_POINT('Ctrl Pts',(42.3965812101076,28.4164594546924,1.497527271977E-15));
#12476=CARTESIAN_POINT('Ctrl Pts',(42.4157719782446,28.4529477707348,1.41553435639707E-15));
#12477=CARTESIAN_POINT('Ctrl Pts',(42.4294374159861,28.4789305145004,1.35714851821164E-15));
#12478=CARTESIAN_POINT('Ctrl Pts',(42.4427062131283,28.5051284836637,-1.16909168511305E-15));
#12479=CARTESIAN_POINT('Ctrl Pts',(42.4555678459356,28.5315352394017,-1.22124532708767E-15));
#12480=CARTESIAN_POINT('Ctrl Pts',(42.4611833798773,28.5430647267815,-1.24401619538084E-15));
#12481=CARTESIAN_POINT('Ctrl Pts',(42.4667203683547,28.5546322173608,-3.62400600888861E-15));
#12482=CARTESIAN_POINT('Ctrl Pts',(42.4721742413373,28.5662288988632,-3.58046925441613E-15));
#12483=CARTESIAN_POINT('Ctrl Pts',(42.5124020601376,28.6517661315138,-3.2593417408755E-15));
#12484=CARTESIAN_POINT('Ctrl Pts',(42.5481738402567,28.7390164875486,-2.58757764947659E-15));
#12485=CARTESIAN_POINT('Ctrl Pts',(42.579238603008,28.8277426426815,-2.27595720048157E-15));
#12486=CARTESIAN_POINT('Ctrl Pts',(42.6096166541956,28.914507434799,-1.9712253721258E-15));
#12487=CARTESIAN_POINT('Ctrl Pts',(42.6354937100697,29.0026841743411,-3.11366339761014E-15));
#12488=CARTESIAN_POINT('Ctrl Pts',(42.6565859526616,29.0920597462289,-2.4980018054066E-15));
#12489=CARTESIAN_POINT('Ctrl Pts',(42.6603145497727,29.1078591804377,-2.3891677625531E-15));
#12490=CARTESIAN_POINT('Ctrl Pts',(42.6638934918523,29.1236960859658,-2.40323005146812E-15));
#12491=CARTESIAN_POINT('Ctrl Pts',(42.6673210388351,29.1395692911278,-2.44249065417534E-15));
#12492=CARTESIAN_POINT('Ctrl Pts',(42.6874319440653,29.2327042725931,-2.69846234523205E-15));
#12493=CARTESIAN_POINT('Ctrl Pts',(42.7023348850078,29.3270899757285,5.17921855384608E-16));
#12494=CARTESIAN_POINT('Ctrl Pts',(42.7121083522879,29.4223175075911,1.0547118733939E-15));
#12495=CARTESIAN_POINT('Ctrl Pts',(42.7153862477415,29.4542555992424,1.23474435409905E-15));
#12496=CARTESIAN_POINT('Ctrl Pts',(42.7180867399261,29.4862882624031,5.37260594040857E-15));
#12497=CARTESIAN_POINT('Ctrl Pts',(42.720211565166,29.5183996018163,5.57887069874141E-15));
#12498=CARTESIAN_POINT('Ctrl Pts',(42.7214001886652,29.5363626285634,5.69425484149674E-15));
#12499=CARTESIAN_POINT('Ctrl Pts',(42.7224086601406,29.5543502699134,1.55024646972868E-15));
#12500=CARTESIAN_POINT('Ctrl Pts',(42.723237204183,29.5723596984032,1.47104550762833E-15));
#12501=CARTESIAN_POINT('Ctrl Pts',(42.7238114727046,29.5848421342712,1.41615087670374E-15));
#12502=CARTESIAN_POINT('Ctrl Pts',(42.7242991897067,29.5973335071231,2.07382757185176E-15));
#12503=CARTESIAN_POINT('Ctrl Pts',(42.7247003050432,29.6098233953396,1.9151347174784E-15));
#12504=CARTESIAN_POINT('Ctrl Pts',(42.7276931454214,29.7030141521449,7.31080309441068E-16));
#12505=CARTESIAN_POINT('Ctrl Pts',(42.7258764010177,29.7962693466217,3.12007103598847E-15));
#12506=CARTESIAN_POINT('Ctrl Pts',(42.7193891741356,29.8892138535835,2.55351295663786E-15));
#12507=CARTESIAN_POINT('Ctrl Pts',(42.7128889885514,29.98234402388,1.9858231367923E-15));
#12508=CARTESIAN_POINT('Ctrl Pts',(42.7016992591496,30.0751632458046,4.70096370999443E-15));
#12509=CARTESIAN_POINT('Ctrl Pts',(42.6859088780022,30.167282139709,4.42701431069281E-15));
#12510=CARTESIAN_POINT('Ctrl Pts',(42.6703416011653,30.2580994740049,4.15693557741601E-15));
#12511=CARTESIAN_POINT('Ctrl Pts',(42.6503022926889,30.3482369776061,1.17383405232967E-15));
#12512=CARTESIAN_POINT('Ctrl Pts',(42.6258330826424,30.4372963921836,1.0547118733939E-15));
#12513=CARTESIAN_POINT('Ctrl Pts',(42.6163194141826,30.4719228366785,1.00839697747183E-15));
#12514=CARTESIAN_POINT('Ctrl Pts',(42.6061356639453,30.5063859711879,9.2547699939467E-16));
#12515=CARTESIAN_POINT('Ctrl Pts',(42.5952827413713,30.5406609260158,7.49400541621981E-16));
#12516=CARTESIAN_POINT('Ctrl Pts',(42.58947852925,30.5589913901751,6.55233730470628E-16));
#12517=CARTESIAN_POINT('Ctrl Pts',(42.5834829076199,30.5772680160108,3.29288427622413E-15));
#12518=CARTESIAN_POINT('Ctrl Pts',(42.577295919888,30.5954868850076,3.24740234702858E-15));
#12519=CARTESIAN_POINT('Ctrl Pts',(42.571847351845,30.6115313240298,3.20734870595345E-15));
#12520=CARTESIAN_POINT('Ctrl Pts',(42.5662498919579,30.6275320443365,4.55710478188197E-15));
#12521=CARTESIAN_POINT('Ctrl Pts',(42.5605096912869,30.6434699599801,4.64905891561784E-15));
#12522=CARTESIAN_POINT('Ctrl Pts',(42.5280842400256,30.7335006290329,5.16849272161559E-15));
#12523=CARTESIAN_POINT('Ctrl Pts',(42.4910677443556,30.8216525646335,2.77315752414307E-15));
#12524=CARTESIAN_POINT('Ctrl Pts',(42.4495332377758,30.9074812017073,1.32532873564628E-15));
#12525=CARTESIAN_POINT('Ctrl Pts',(42.4183823578409,30.9718526795127,2.39457144273687E-16));
#12526=CARTESIAN_POINT('Ctrl Pts',(42.3846889484228,31.0349167649365,4.76029285454196E-15));
#12527=CARTESIAN_POINT('Ctrl Pts',(42.3484664521773,31.0964687502367,5.23192600354605E-15));
#12528=CARTESIAN_POINT('Ctrl Pts',(42.333534659064,31.1218419742131,5.42634464765648E-15));
#12529=CARTESIAN_POINT('Ctrl Pts',(42.3181729379481,31.1469580489284,6.86998275533235E-15));
#12530=CARTESIAN_POINT('Ctrl Pts',(42.3023815725951,31.1718017291815,6.78623823802127E-15));
#12531=CARTESIAN_POINT('Ctrl Pts',(42.2929489473471,31.1866415559078,6.73621528999162E-15));
#12532=CARTESIAN_POINT('Ctrl Pts',(42.2833677032904,31.2013767722444,5.84885791077277E-15));
#12533=CARTESIAN_POINT('Ctrl Pts',(42.2736398792402,31.2160020566235,5.75234304633909E-15));
#12534=CARTESIAN_POINT('Ctrl Pts',(42.2261111879894,31.2874590054872,5.28078587496221E-15));
#12535=CARTESIAN_POINT('Ctrl Pts',(42.175073702515,31.3563139832513,4.49466789804242E-15));
#12536=CARTESIAN_POINT('Ctrl Pts',(42.1205618043097,31.4222142805125,2.85188539450587E-15));
#12537=CARTESIAN_POINT('Ctrl Pts',(42.0689758173165,31.48457739736,1.29727879209382E-15));
#12538=CARTESIAN_POINT('Ctrl Pts',(42.0142778931532,31.5442947238755,-1.0060863342509E-15));
#12539=CARTESIAN_POINT('Ctrl Pts',(41.9564733781692,31.6010314766203,-2.0491421059976E-15));
#12540=CARTESIAN_POINT('Ctrl Pts',(41.9435074061502,31.6137579418236,-2.32930748699949E-15));
#12541=CARTESIAN_POINT('Ctrl Pts',(41.9303850442016,31.6263342844393,2.04314546332945E-17));
#12542=CARTESIAN_POINT('Ctrl Pts',(41.9171095224698,31.6387591744824,2.77555756156289E-17));
#12543=CARTESIAN_POINT('Ctrl Pts',(37.4805317771007,29.9980220368919,8.38741669750803));
#12544=CARTESIAN_POINT('Ctrl Pts',(37.4794102776092,29.8678903638642,8.39566206758641));
#12545=CARTESIAN_POINT('Ctrl Pts',(37.4886217757044,29.7379179497287,8.40390743766479));
#12546=CARTESIAN_POINT('Ctrl Pts',(37.5087192791305,29.6096513413884,8.41215280774317));
#12547=CARTESIAN_POINT('Ctrl Pts',(37.6377281009826,28.7862891717617,8.46508104748506));
#12548=CARTESIAN_POINT('Ctrl Pts',(38.2152996031925,28.0332154868897,8.51800928722696));
#12549=CARTESIAN_POINT('Ctrl Pts',(38.977056194255,27.6951309495556,8.57093752696885));
#12550=CARTESIAN_POINT('Ctrl Pts',(39.7388127853175,27.3570464122215,8.62386576671075));
#12551=CARTESIAN_POINT('Ctrl Pts',(40.6847544652325,27.4339510224254,8.67679400645264));
#12552=CARTESIAN_POINT('Ctrl Pts',(41.3818822592687,27.8906674923104,8.72972224619453));
#12553=CARTESIAN_POINT('Ctrl Pts',(42.0790100533048,28.3473839621954,8.78265048593643));
#12554=CARTESIAN_POINT('Ctrl Pts',(42.527323961462,29.1839122917617,8.83557872567833));
#12555=CARTESIAN_POINT('Ctrl Pts',(42.5216159580211,30.0172882838724,8.88850696542022));
#12556=CARTESIAN_POINT('Ctrl Pts',(42.5159079545802,30.8506642759831,8.94143520516211));
#12557=CARTESIAN_POINT('Ctrl Pts',(42.0561780395411,31.6808879306382,8.994363444904));
#12558=CARTESIAN_POINT('Ctrl Pts',(41.3528558686579,32.1280316339289,9.0472916846459));
#12559=CARTESIAN_POINT('Ctrl Pts',(40.6495336977747,32.5751753372196,9.10021992438779));
#12560=CARTESIAN_POINT('Ctrl Pts',(39.7026192710474,32.6392390891458,9.15314816412969));
#12561=CARTESIAN_POINT('Ctrl Pts',(38.9455706527587,32.2906976513646,9.20607640387159));
#12562=CARTESIAN_POINT('Ctrl Pts',(38.1885220344699,31.9421562135835,9.25900464361348));
#12563=CARTESIAN_POINT('Ctrl Pts',(37.6213392246197,31.181009586095,9.31193288335538));
#12564=CARTESIAN_POINT('Ctrl Pts',(37.5036139674033,30.3560672289173,9.36486112309727));
#12565=CARTESIAN_POINT('Ctrl Pts',(37.4868909425926,30.2388831018008,9.37237964790086));
#12566=CARTESIAN_POINT('Ctrl Pts',(37.4792373281869,30.1204116681271,9.37989817270444));
#12567=CARTESIAN_POINT('Ctrl Pts',(37.480218046669,30.0018167092234,9.38741669750803));
#12568=CARTESIAN_POINT('Ctrl Pts',(39.2062007174671,27.0307770462543,10.));
#12569=CARTESIAN_POINT('Ctrl Pts',(38.2187620536724,27.2947612990625,9.94707176025811));
#12570=CARTESIAN_POINT('Ctrl Pts',(36.5451697653868,28.8815756987713,9.84121528077432));
#12571=CARTESIAN_POINT('Ctrl Pts',(37.1870303021875,32.3023719893123,9.68243056154863));
#12572=CARTESIAN_POINT('Ctrl Pts',(40.4091142878593,33.6090240981732,9.52364584232295));
#12573=CARTESIAN_POINT('Ctrl Pts',(43.2541895529164,31.6147492063695,9.36486112309727));
#12574=CARTESIAN_POINT('Ctrl Pts',(43.1213435063924,28.1406673653848,9.20607640387158));
#12575=CARTESIAN_POINT('Ctrl Pts',(40.1303404706603,26.3695397560852,9.0472916846459));
#12576=CARTESIAN_POINT('Ctrl Pts',(37.0203226655434,27.9216549951598,8.88850696542021));
#12577=CARTESIAN_POINT('Ctrl Pts',(36.6379950966727,31.3766528296008,8.72972224619454));
#12578=CARTESIAN_POINT('Ctrl Pts',(39.3336051768584,33.5712515449036,8.57093752696884));
#12579=CARTESIAN_POINT('Ctrl Pts',(42.63924979695,32.4964766410994,8.41215280774317));
#12580=CARTESIAN_POINT('Ctrl Pts',(43.5287243142158,29.1361944846783,8.25336808851748));
#12581=CARTESIAN_POINT('Ctrl Pts',(41.1877002535156,26.5667240916348,8.0945833692918));
#12582=CARTESIAN_POINT('Ctrl Pts',(37.7593611185253,27.1403550261585,7.93579865006611));
#12583=CARTESIAN_POINT('Ctrl Pts',(36.3822874180148,30.3319467259865,7.77701393084044));
#12584=CARTESIAN_POINT('Ctrl Pts',(38.3171710506372,33.2196451638042,7.61822921161474));
#12585=CARTESIAN_POINT('Ctrl Pts',(41.7926561734374,33.159812400248,7.45944449238906));
#12586=CARTESIAN_POINT('Ctrl Pts',(43.6269944901785,30.207223201086,7.30065977316338));
#12587=CARTESIAN_POINT('Ctrl Pts',(42.1408791121553,27.0649247751536,7.14187505393769));
#12588=CARTESIAN_POINT('Ctrl Pts',(38.6948243496615,26.6096391370258,6.98309033471202));
#12589=CARTESIAN_POINT('Ctrl Pts',(36.4436362959865,29.2581729107715,6.82430561548632));
#12590=CARTESIAN_POINT('Ctrl Pts',(37.4482404844472,32.5858371063758,6.66552089626065));
#12591=CARTESIAN_POINT('Ctrl Pts',(40.7889383467181,33.5462101590121,6.50673617703496));
#12592=CARTESIAN_POINT('Ctrl Pts',(43.4073761900399,31.2600863855708,6.34795145780928));
#12593=CARTESIAN_POINT('Ctrl Pts',(42.9064174160314,27.8203743447495,6.1891667385836));
#12594=CARTESIAN_POINT('Ctrl Pts',(39.7446815105131,26.3760735841615,6.03038201935791));
#12595=CARTESIAN_POINT('Ctrl Pts',(36.816685463857,28.2494175937138,5.87159730013222));
#12596=CARTESIAN_POINT('Ctrl Pts',(36.8029612895799,31.7253908776466,5.71281258090655));
#12597=CARTESIAN_POINT('Ctrl Pts',(39.7160732420625,33.6217973153363,5.55402786168086));
#12598=CARTESIAN_POINT('Ctrl Pts',(42.8891154512744,32.2025081398842,5.39524314245518));
#12599=CARTESIAN_POINT('Ctrl Pts',(43.4172201906419,28.7668591460577,5.23645842322949));
#12600=CARTESIAN_POINT('Ctrl Pts',(40.8169162951919,26.4601302335076,5.07767370400381));
#12601=CARTESIAN_POINT('Ctrl Pts',(37.4687390262765,27.3940936164278,4.91888898477813));
#12602=CARTESIAN_POINT('Ctrl Pts',(36.4378893644385,30.7137212460463,4.76010426555244));
#12603=CARTESIAN_POINT('Ctrl Pts',(38.6680931462871,33.3799488650141,4.60131954632676));
#12604=CARTESIAN_POINT('Ctrl Pts',(42.1176356506926,32.9518891320487,4.44253482710108));
#12605=CARTESIAN_POINT('Ctrl Pts',(43.6285176985082,29.8214236615297,4.28375010787539));
#12606=CARTESIAN_POINT('Ctrl Pts',(41.8175517334939,26.8544418788833,4.1249653886497));
#12607=CARTESIAN_POINT('Ctrl Pts',(38.3426471809504,26.7671665941811,3.96618066942403));
#12608=CARTESIAN_POINT('Ctrl Pts',(36.3850217561086,29.639496888487,3.80739595019834));
#12609=CARTESIAN_POINT('Ctrl Pts',(37.7368491970887,32.8418618266495,3.64861123097266));
#12610=CARTESIAN_POINT('Ctrl Pts',(41.1605538126502,33.4425492067914,3.48982651174697));
#12611=CARTESIAN_POINT('Ctrl Pts',(43.5217905842841,30.8916396581577,3.33104179252129));
#12612=CARTESIAN_POINT('Ctrl Pts',(42.6588862528215,27.5244487277861,3.17225707329561));
#12613=CARTESIAN_POINT('Ctrl Pts',(39.3618154801332,26.4235841007334,3.01347235406992));
#12614=CARTESIAN_POINT('Ctrl Pts',(36.6489920919044,28.5968691346069,2.85468763484424));
#12615=CARTESIAN_POINT('Ctrl Pts',(37.0039610899898,32.0546973278633,2.69590291561856));
#12616=CARTESIAN_POINT('Ctrl Pts',(40.1017542133218,33.6314839980979,2.53711819639287));
#12617=CARTESIAN_POINT('Ctrl Pts',(43.1063930447263,31.883707179614,2.37833347716719));
#12618=CARTESIAN_POINT('Ctrl Pts',(43.2671803398556,28.4114273111418,2.21954875794151));
#12619=CARTESIAN_POINT('Ctrl Pts',(40.4369180427711,26.3934599853152,2.06076403871582));
#12620=CARTESIAN_POINT('Ctrl Pts',(37.2066644196549,27.6772194915737,1.90197931949014));
#12621=CARTESIAN_POINT('Ctrl Pts',(36.5336635272788,31.0874481281771,1.74319460026446));
#12622=CARTESIAN_POINT('Ctrl Pts',(39.0340361139851,33.5021320828999,1.58440988103877));
#12623=CARTESIAN_POINT('Ctrl Pts',(42.4187332816925,32.7106797239938,1.42562516181309));
#12624=CARTESIAN_POINT('Ctrl Pts',(43.5891188868934,29.4376293695436,1.2668404425874));
#12625=CARTESIAN_POINT('Ctrl Pts',(41.4737278337939,26.6794509596774,1.10805572336172));
#12626=CARTESIAN_POINT('Ctrl Pts',(38.0091585148051,26.9611185998674,0.949271004136034));
#12627=CARTESIAN_POINT('Ctrl Pts',(36.3671812304715,30.0249552475435,0.790486284910356));
#12628=CARTESIAN_POINT('Ctrl Pts',(38.0509704657541,33.0656996094815,0.631701565684668));
#12629=CARTESIAN_POINT('Ctrl Pts',(41.5191020833988,33.300338163167,0.472916846458987));
#12630=CARTESIAN_POINT('Ctrl Pts',(43.5964449208384,30.5125900673602,0.314132127233303));
#12631=CARTESIAN_POINT('Ctrl Pts',(42.3814529285809,27.2575355260863,0.155347408007619));
#12632=CARTESIAN_POINT('Ctrl Pts',(38.9859852522992,26.509227966563,-0.00343731121806271));
#12633=CARTESIAN_POINT('Ctrl Pts',(36.5193457296438,28.9647364017664,-0.162222030443748));
#12634=CARTESIAN_POINT('Ctrl Pts',(36.9997188544053,31.2204253757917,-0.268078509927537));
#12635=CARTESIAN_POINT('Ctrl Pts',(37.6639373423039,31.9973015569307,-0.321006749669432));
#12636=CARTESIAN_POINT('Ctrl Pts',(39.254067145653,27.2098224301579,10.1070022498898));
#12637=CARTESIAN_POINT('Ctrl Pts',(38.326171445588,27.4578883222957,10.0540740101479));
#12638=CARTESIAN_POINT('Ctrl Pts',(36.753497471091,28.9490171511311,9.94821753066412));
#12639=CARTESIAN_POINT('Ctrl Pts',(37.3566535495151,32.1635379970062,9.78943281143845));
#12640=CARTESIAN_POINT('Ctrl Pts',(40.3844445254766,33.391398438113,9.63064809221276));
#12641=CARTESIAN_POINT('Ctrl Pts',(43.0579605640956,31.5173791549904,9.47186337298707));
#12642=CARTESIAN_POINT('Ctrl Pts',(42.9331251896467,28.2527858996124,9.31307865376139));
#12643=CARTESIAN_POINT('Ctrl Pts',(40.1224808858561,26.5884580246842,9.15429393453571));
#12644=CARTESIAN_POINT('Ctrl Pts',(37.199998452969,28.0469800667601,8.99550921531002));
#12645=CARTESIAN_POINT('Ctrl Pts',(36.8407253961413,31.2936400891575,8.83672449608435));
#12646=CARTESIAN_POINT('Ctrl Pts',(39.3737890629457,33.3559035855774,8.67793977685866));
#12647=CARTESIAN_POINT('Ctrl Pts',(42.4801019321808,32.3459380572427,8.51915505763298));
#12648=CARTESIAN_POINT('Ctrl Pts',(43.3159407646573,29.1882823179323,8.36037033840729));
#12649=CARTESIAN_POINT('Ctrl Pts',(41.116081432307,26.7737520624662,8.20158561918161));
#12650=CARTESIAN_POINT('Ctrl Pts',(37.8944725786522,27.3127928121198,8.04280089995593));
#12651=CARTESIAN_POINT('Ctrl Pts',(36.6004369972767,30.3119301998059,7.88401618073024));
#12652=CARTESIAN_POINT('Ctrl Pts',(38.4186463389453,33.0254992160709,7.72523146150456));
#12653=CARTESIAN_POINT('Ctrl Pts',(41.6845582576594,32.9692743931401,7.56644674227887));
#12654=CARTESIAN_POINT('Ctrl Pts',(43.408285207977,30.194727555535,7.40766202305319));
#12655=CARTESIAN_POINT('Ctrl Pts',(42.0117832077729,27.2419110367462,7.24887730382751));
#12656=CARTESIAN_POINT('Ctrl Pts',(38.7735269863502,26.8140793127011,7.09009258460182));
#12657=CARTESIAN_POINT('Ctrl Pts',(36.6580865122905,29.3029053940003,6.93130786537614));
#12658=CARTESIAN_POINT('Ctrl Pts',(37.6021126487167,32.4299100491507,6.77252314615045));
#12659=CARTESIAN_POINT('Ctrl Pts',(40.7413650349914,33.3323722057112,6.61373842692478));
#12660=CARTESIAN_POINT('Ctrl Pts',(43.2019099830379,31.1841026503746,6.45495370769908));
#12661=CARTESIAN_POINT('Ctrl Pts',(42.7311592322764,27.9518066818591,6.29616898847341));
#12662=CARTESIAN_POINT('Ctrl Pts',(39.7600773220368,26.5945978601993,6.13738426924772));
#12663=CARTESIAN_POINT('Ctrl Pts',(37.0086406595725,28.3549784437647,5.97859955002205));
#12664=CARTESIAN_POINT('Ctrl Pts',(36.9957440587349,31.6213490872912,5.81981483079635));
#12665=CARTESIAN_POINT('Ctrl Pts',(39.7331941441191,33.4034014249478,5.66103011157068));
#12666=CARTESIAN_POINT('Ctrl Pts',(42.7149005832186,32.0696959793966,5.50224539234498));
#12667=CARTESIAN_POINT('Ctrl Pts',(43.2111603862932,28.8412180544458,5.34346067311931));
#12668=CARTESIAN_POINT('Ctrl Pts',(40.7676559014902,26.6735858584921,5.18467595389361));
#12669=CARTESIAN_POINT('Ctrl Pts',(37.6213751199146,27.5512308594478,5.02589123466794));
#12670=CARTESIAN_POINT('Ctrl Pts',(36.6526861231145,30.6706835568969,4.86710651544225));
#12671=CARTESIAN_POINT('Ctrl Pts',(38.7484076857008,33.1761365371633,4.70832179621658));
#12672=CARTESIAN_POINT('Ctrl Pts',(41.9899413367417,32.7738889848312,4.54953707699088));
#12673=CARTESIAN_POINT('Ctrl Pts',(43.4097165662084,29.8321918893037,4.39075235776521));
#12674=CARTESIAN_POINT('Ctrl Pts',(41.7079526050494,27.0441203470077,4.23196763853952));
#12675=CARTESIAN_POINT('Ctrl Pts',(38.4425862479632,26.9621077984146,4.07318291931383));
#12676=CARTESIAN_POINT('Ctrl Pts',(36.6030064536416,29.6612353766385,3.91439820008815));
#12677=CARTESIAN_POINT('Ctrl Pts',(37.873318135478,32.6704963718892,3.75561348086247));
#12678=CARTESIAN_POINT('Ctrl Pts',(41.0905719331606,33.2349620521929,3.59682876163679));
#12679=CARTESIAN_POINT('Ctrl Pts',(43.3094251415357,30.8378734144685,3.43804404241111));
#12680=CARTESIAN_POINT('Ctrl Pts',(42.498554301564,27.6737255031617,3.27925932318542));
#12681=CARTESIAN_POINT('Ctrl Pts',(39.4002982731538,26.6392434727839,3.12047460395974));
#12682=CARTESIAN_POINT('Ctrl Pts',(36.8510592679687,28.6814785116644,2.96168988473405));
#12683=CARTESIAN_POINT('Ctrl Pts',(37.1846234872531,31.9307982210587,2.80290516550837));
#12684=CARTESIAN_POINT('Ctrl Pts',(40.0956183917712,33.4125039966943,2.64412044628268));
#12685=CARTESIAN_POINT('Ctrl Pts',(42.9190762470616,31.7701188501454,2.485335727057));
#12686=CARTESIAN_POINT('Ctrl Pts',(43.0701680011581,28.5072189075851,2.32655100783132));
#12687=CARTESIAN_POINT('Ctrl Pts',(40.4105717023578,26.6109358541037,2.16776628860563));
#12688=CARTESIAN_POINT('Ctrl Pts',(37.3751037215009,27.8172841261039,2.00898156937995));
#12689=CARTESIAN_POINT('Ctrl Pts',(36.7426850639453,31.0218745519863,1.85019685015427));
#12690=CARTESIAN_POINT('Ctrl Pts',(39.092284139648,33.2909520559933,1.69141213092858));
#12691=CARTESIAN_POINT('Ctrl Pts',(42.2728826548695,32.5472246047984,1.5326274117029));
#12692=CARTESIAN_POINT('Ctrl Pts',(43.3726935193849,29.4715405533769,1.37384269247721));
#12693=CARTESIAN_POINT('Ctrl Pts',(41.3848614300641,26.879681453297,1.21505797325153));
#12694=CARTESIAN_POINT('Ctrl Pts',(38.129207087634,27.1443644171738,1.05627325402585));
#12695=CARTESIAN_POINT('Ctrl Pts',(36.5862417191497,30.0234504356966,0.897488534800165));
#12696=CARTESIAN_POINT('Ctrl Pts',(38.1684977604822,32.8808366429534,0.73870381557448));
#12697=CARTESIAN_POINT('Ctrl Pts',(41.4274995934721,33.1013263938789,0.579919096348797));
#12698=CARTESIAN_POINT('Ctrl Pts',(43.379577790424,30.4816806722675,0.421134377123115));
#12699=CARTESIAN_POINT('Ctrl Pts',(42.2378503226169,27.4229072789734,0.262349657897429));
#12700=CARTESIAN_POINT('Ctrl Pts',(39.0471307649853,26.7197229777436,0.103564938671748));
#12701=CARTESIAN_POINT('Ctrl Pts',(36.729230635486,29.027163229012,-0.0552197805539379));
#12702=CARTESIAN_POINT('Ctrl Pts',(37.1806370602456,31.1468332160454,-0.161076260037726));
#12703=CARTESIAN_POINT('Ctrl Pts',(37.8048028959809,31.8768634390788,-0.214004499779622));
#12704=CARTESIAN_POINT('Ctrl Pts',(39.301933573839,27.3888678140614,10.2140044997796));
#12705=CARTESIAN_POINT('Ctrl Pts',(38.4335808375037,27.6210153455288,10.1610762600377));
#12706=CARTESIAN_POINT('Ctrl Pts',(36.9618251767951,29.0164586034908,10.0552197805539));
#12707=CARTESIAN_POINT('Ctrl Pts',(37.5262767968427,32.0247040047002,9.89643506132825));
#12708=CARTESIAN_POINT('Ctrl Pts',(40.3597747630939,33.1737727780529,9.73765034210257));
#12709=CARTESIAN_POINT('Ctrl Pts',(42.8617315752749,31.4200091036112,9.57886562287689));
#12710=CARTESIAN_POINT('Ctrl Pts',(42.7449068729009,28.3649044338401,9.4200809036512));
#12711=CARTESIAN_POINT('Ctrl Pts',(40.1146213010519,26.8073762932831,9.26129618442552));
#12712=CARTESIAN_POINT('Ctrl Pts',(37.3796742403946,28.1723051383605,9.10251146519983));
#12713=CARTESIAN_POINT('Ctrl Pts',(37.0434556956098,31.2106273487141,8.94372674597416));
#12714=CARTESIAN_POINT('Ctrl Pts',(39.4139729490328,33.1405556262513,8.78494202674846));
#12715=CARTESIAN_POINT('Ctrl Pts',(42.3209540674116,32.1953994733859,8.62615730752279));
#12716=CARTESIAN_POINT('Ctrl Pts',(43.1031572150988,29.2403701511864,8.4673725882971));
#12717=CARTESIAN_POINT('Ctrl Pts',(41.0444626110982,26.9807800332976,8.30858786907142));
#12718=CARTESIAN_POINT('Ctrl Pts',(38.0295840387791,27.4852305980811,8.14980314984573));
#12719=CARTESIAN_POINT('Ctrl Pts',(36.8185865765384,30.2919136736252,7.99101843062005));
#12720=CARTESIAN_POINT('Ctrl Pts',(38.5201216272536,32.8313532683376,7.83223371139437));
#12721=CARTESIAN_POINT('Ctrl Pts',(41.5764603418814,32.7787363860323,7.67344899216869));
#12722=CARTESIAN_POINT('Ctrl Pts',(43.1895759257755,30.1822319099838,7.514664272943));
#12723=CARTESIAN_POINT('Ctrl Pts',(41.8826873033904,27.4188972983388,7.35587955371731));
#12724=CARTESIAN_POINT('Ctrl Pts',(38.8522296230389,27.0185194883763,7.19709483449164));
#12725=CARTESIAN_POINT('Ctrl Pts',(36.8725367285946,29.3476378772291,7.03831011526595));
#12726=CARTESIAN_POINT('Ctrl Pts',(37.7559848129862,32.2739829919254,6.87952539604026));
#12727=CARTESIAN_POINT('Ctrl Pts',(40.6937917232649,33.1185342524103,6.7207406768146));
#12728=CARTESIAN_POINT('Ctrl Pts',(42.9964437760359,31.1081189151782,6.56195595758889));
#12729=CARTESIAN_POINT('Ctrl Pts',(42.5559010485213,28.0832390189687,6.40317123836322));
#12730=CARTESIAN_POINT('Ctrl Pts',(39.7754731335606,26.813122136237,6.24438651913753));
#12731=CARTESIAN_POINT('Ctrl Pts',(37.2005958552881,28.4605392938157,6.08560179991186));
#12732=CARTESIAN_POINT('Ctrl Pts',(37.1885268278899,31.5173072969359,5.92681708068615));
#12733=CARTESIAN_POINT('Ctrl Pts',(39.7503150461758,33.1850055345593,5.7680323614605));
#12734=CARTESIAN_POINT('Ctrl Pts',(42.5406857151627,31.9368838189091,5.60924764223479));
#12735=CARTESIAN_POINT('Ctrl Pts',(43.0051005819446,28.9155769628338,5.45046292300913));
#12736=CARTESIAN_POINT('Ctrl Pts',(40.7183955077885,26.8870414834766,5.29167820378342));
#12737=CARTESIAN_POINT('Ctrl Pts',(37.7740112135527,27.7083681024678,5.13289348455775));
#12738=CARTESIAN_POINT('Ctrl Pts',(36.8674828817906,30.6276458677476,4.97410876533206));
#12739=CARTESIAN_POINT('Ctrl Pts',(38.8287222251146,32.9723242093125,4.81532404610638));
#12740=CARTESIAN_POINT('Ctrl Pts',(41.8622470227907,32.5958888376137,4.65653932688069));
#12741=CARTESIAN_POINT('Ctrl Pts',(43.1909154339085,29.8429601170776,4.49775460765501));
#12742=CARTESIAN_POINT('Ctrl Pts',(41.5983534766049,27.2337988151321,4.33896988842933));
#12743=CARTESIAN_POINT('Ctrl Pts',(38.542525314976,27.1570490026481,4.18018516920365));
#12744=CARTESIAN_POINT('Ctrl Pts',(36.8209911511747,29.6829738647901,4.02140044997796));
#12745=CARTESIAN_POINT('Ctrl Pts',(38.0097870738674,32.4991309171289,3.86261573075228));
#12746=CARTESIAN_POINT('Ctrl Pts',(41.020590053671,33.0273748975943,3.70383101152659));
#12747=CARTESIAN_POINT('Ctrl Pts',(43.0970596987873,30.7841071707794,3.54504629230091));
#12748=CARTESIAN_POINT('Ctrl Pts',(42.3382223503066,27.8230022785374,3.38626157307523));
#12749=CARTESIAN_POINT('Ctrl Pts',(39.4387810661743,26.8549028448345,3.22747685384954));
#12750=CARTESIAN_POINT('Ctrl Pts',(37.053126444033,28.7660878887219,3.06869213462386));
#12751=CARTESIAN_POINT('Ctrl Pts',(37.3652858845164,31.8068991142541,2.90990741539818));
#12752=CARTESIAN_POINT('Ctrl Pts',(40.0894825702206,33.1935239952906,2.75112269617249));
#12753=CARTESIAN_POINT('Ctrl Pts',(42.7317594493968,31.6565305206768,2.59233797694681));
#12754=CARTESIAN_POINT('Ctrl Pts',(42.8731556624607,28.6030105040283,2.43355325772113));
#12755=CARTESIAN_POINT('Ctrl Pts',(40.3842253619445,26.8284117228923,2.27476853849544));
#12756=CARTESIAN_POINT('Ctrl Pts',(37.543543023347,27.957348760634,2.11598381926976));
#12757=CARTESIAN_POINT('Ctrl Pts',(36.9517066006117,30.9563009757956,1.95719910004408));
#12758=CARTESIAN_POINT('Ctrl Pts',(39.1505321653109,33.0797720290867,1.79841438081839));
#12759=CARTESIAN_POINT('Ctrl Pts',(42.1270320280466,32.3837694856031,1.63962966159271));
#12760=CARTESIAN_POINT('Ctrl Pts',(43.1562681518763,29.50545173721,1.48084494236703));
#12761=CARTESIAN_POINT('Ctrl Pts',(41.2959950263345,27.0799119469166,1.32206022314134));
#12762=CARTESIAN_POINT('Ctrl Pts',(38.2492556604628,27.3276102344802,1.16327550391566));
#12763=CARTESIAN_POINT('Ctrl Pts',(36.805302207828,30.0219456238497,1.00449078468998));
#12764=CARTESIAN_POINT('Ctrl Pts',(38.2860250552103,32.6959736764254,0.845706065464291));
#12765=CARTESIAN_POINT('Ctrl Pts',(41.3358971035453,32.9023146245908,0.686921346238608));
#12766=CARTESIAN_POINT('Ctrl Pts',(43.1627106600096,30.4507712771748,0.528136627012925));
#12767=CARTESIAN_POINT('Ctrl Pts',(42.0942477166529,27.5882790318606,0.36935190778724));
#12768=CARTESIAN_POINT('Ctrl Pts',(39.1082762776713,26.9302179889242,0.210567188561559));
#12769=CARTESIAN_POINT('Ctrl Pts',(36.9391155413282,29.0895900562576,0.051782469335873));
#12770=CARTESIAN_POINT('Ctrl Pts',(37.3615552660859,31.0732410562992,-0.0540740101479155));
#12771=CARTESIAN_POINT('Ctrl Pts',(37.9456684496579,31.7564253212269,-0.107002249889811));
#12772=CARTESIAN_POINT('Ctrl Pts',(39.3498000020249,27.5679131979649,10.3210067496694));
#12773=CARTESIAN_POINT('Ctrl Pts',(38.5409902294193,27.784142368762,10.2680785099275));
#12774=CARTESIAN_POINT('Ctrl Pts',(37.1701528824992,29.0839000558506,10.1622220304438));
#12775=CARTESIAN_POINT('Ctrl Pts',(37.6959000441702,31.8858700123942,10.0034373112181));
#12776=CARTESIAN_POINT('Ctrl Pts',(40.3351050007111,32.9561471179928,9.84465259199238));
#12777=CARTESIAN_POINT('Ctrl Pts',(42.6655025864542,31.3226390522321,9.6858678727667));
#12778=CARTESIAN_POINT('Ctrl Pts',(42.5566885561551,28.4770229680677,9.52708315354102));
#12779=CARTESIAN_POINT('Ctrl Pts',(40.1067617162477,27.0262945618821,9.36829843431533));
#12780=CARTESIAN_POINT('Ctrl Pts',(37.5593500278202,28.2976302099609,9.20951371508965));
#12781=CARTESIAN_POINT('Ctrl Pts',(37.2461859950784,31.1276146082707,9.05072899586396));
#12782=CARTESIAN_POINT('Ctrl Pts',(39.45415683512,32.9252076669253,8.89194427663829));
#12783=CARTESIAN_POINT('Ctrl Pts',(42.1618062026424,32.0448608895291,8.73315955741259));
#12784=CARTESIAN_POINT('Ctrl Pts',(42.8903736655403,29.2924579844404,8.57437483818692));
#12785=CARTESIAN_POINT('Ctrl Pts',(40.9728437898896,27.187808004129,8.41559011896122));
#12786=CARTESIAN_POINT('Ctrl Pts',(38.164695498906,27.6576683840423,8.25680539973555));
#12787=CARTESIAN_POINT('Ctrl Pts',(37.0367361558003,30.2718971474446,8.09802068050986));
#12788=CARTESIAN_POINT('Ctrl Pts',(38.6215969155617,32.6372073206043,7.93923596128419));
#12789=CARTESIAN_POINT('Ctrl Pts',(41.4683624261034,32.5881983789245,7.78045124205849));
#12790=CARTESIAN_POINT('Ctrl Pts',(42.9708666435739,30.1697362644327,7.62166652283282));
#12791=CARTESIAN_POINT('Ctrl Pts',(41.753591399008,27.5958835599314,7.46288180360712));
#12792=CARTESIAN_POINT('Ctrl Pts',(38.9309322597276,27.2229596640516,7.30409708438145));
#12793=CARTESIAN_POINT('Ctrl Pts',(37.0869869448986,29.3923703604579,7.14531236515576));
#12794=CARTESIAN_POINT('Ctrl Pts',(37.9098569772558,32.1180559347003,6.98652764593008));
#12795=CARTESIAN_POINT('Ctrl Pts',(40.6462184115382,32.9046962991094,6.8277429267044));
#12796=CARTESIAN_POINT('Ctrl Pts',(42.7909775690338,31.032135179982,6.66895820747871));
#12797=CARTESIAN_POINT('Ctrl Pts',(42.3806428647663,28.2146713560783,6.51017348825303));
#12798=CARTESIAN_POINT('Ctrl Pts',(39.7908689450844,27.0316464122748,6.35138876902734));
#12799=CARTESIAN_POINT('Ctrl Pts',(37.3925510510037,28.5661001438667,6.19260404980166));
#12800=CARTESIAN_POINT('Ctrl Pts',(37.3813095970449,31.4132655065806,6.03381933057598));
#12801=CARTESIAN_POINT('Ctrl Pts',(39.7674359482324,32.9666096441708,5.87503461135029));
#12802=CARTESIAN_POINT('Ctrl Pts',(42.3664708471069,31.8040716584215,5.71624989212461));
#12803=CARTESIAN_POINT('Ctrl Pts',(42.7990407775959,28.9899358712219,5.55746517289892));
#12804=CARTESIAN_POINT('Ctrl Pts',(40.6691351140867,27.1004971084611,5.39868045367324));
#12805=CARTESIAN_POINT('Ctrl Pts',(37.9266473071909,27.8655053454879,5.23989573444756));
#12806=CARTESIAN_POINT('Ctrl Pts',(37.0822796404666,30.5846081785982,5.08111101522187));
#12807=CARTESIAN_POINT('Ctrl Pts',(38.9090367645283,32.7685118814618,4.9223262959962));
#12808=CARTESIAN_POINT('Ctrl Pts',(41.7345527088397,32.4178886903962,4.76354157677051));
#12809=CARTESIAN_POINT('Ctrl Pts',(42.9721143016087,29.8537283448515,4.60475685754483));
#12810=CARTESIAN_POINT('Ctrl Pts',(41.4887543481603,27.4234772832564,4.44597213831914));
#12811=CARTESIAN_POINT('Ctrl Pts',(38.6424643819888,27.3519902068817,4.28718741909346));
#12812=CARTESIAN_POINT('Ctrl Pts',(37.0389758487078,29.7047123529416,4.12840269986777));
#12813=CARTESIAN_POINT('Ctrl Pts',(38.1462560122567,32.3277654623687,3.9696179806421));
#12814=CARTESIAN_POINT('Ctrl Pts',(40.9506081741815,32.8197877429958,3.8108332614164));
#12815=CARTESIAN_POINT('Ctrl Pts',(42.8846942560388,30.7303409270902,3.65204854219072));
#12816=CARTESIAN_POINT('Ctrl Pts',(42.1778903990493,27.972279053913,3.49326382296504));
#12817=CARTESIAN_POINT('Ctrl Pts',(39.4772638591948,27.0705622168851,3.33447910373936));
#12818=CARTESIAN_POINT('Ctrl Pts',(37.2551936200974,28.8506972657794,3.17569438451367));
#12819=CARTESIAN_POINT('Ctrl Pts',(37.5459482817796,31.6830000074495,3.01690966528799));
#12820=CARTESIAN_POINT('Ctrl Pts',(40.0833467486701,32.974543993887,2.8581249460623));
#12821=CARTESIAN_POINT('Ctrl Pts',(42.5444426517321,31.5429421912082,2.69934022683662));
#12822=CARTESIAN_POINT('Ctrl Pts',(42.6761433237633,28.6988021004716,2.54055550761094));
#12823=CARTESIAN_POINT('Ctrl Pts',(40.3578790215312,27.0458875916808,2.38177078838525));
#12824=CARTESIAN_POINT('Ctrl Pts',(37.7119823251932,28.0974133951641,2.22298606915957));
#12825=CARTESIAN_POINT('Ctrl Pts',(37.1607281372782,30.8907273996049,2.06420134993389));
#12826=CARTESIAN_POINT('Ctrl Pts',(39.2087801909737,32.8685920021801,1.9054166307082));
#12827=CARTESIAN_POINT('Ctrl Pts',(41.9811814012236,32.2203143664078,1.74663191148252));
#12828=CARTESIAN_POINT('Ctrl Pts',(42.9398427843677,29.5393629210432,1.58784719225684));
#12829=CARTESIAN_POINT('Ctrl Pts',(41.2071286226048,27.2801424405362,1.42906247303115));
#12830=CARTESIAN_POINT('Ctrl Pts',(38.3693042332916,27.5108560517866,1.27027775380547));
#12831=CARTESIAN_POINT('Ctrl Pts',(37.0243626965063,30.0204408120029,1.11149303457979));
#12832=CARTESIAN_POINT('Ctrl Pts',(38.4035523499385,32.5111107098974,0.952708315354102));
#12833=CARTESIAN_POINT('Ctrl Pts',(41.2442946136185,32.7033028553028,0.793923596128417));
#12834=CARTESIAN_POINT('Ctrl Pts',(42.9458435295952,30.419861882082,0.635138876902737));
#12835=CARTESIAN_POINT('Ctrl Pts',(41.9506451106889,27.7536507847478,0.47635415767705));
#12836=CARTESIAN_POINT('Ctrl Pts',(39.1694217903574,27.1407130001049,0.31756943845137));
#12837=CARTESIAN_POINT('Ctrl Pts',(37.1490004471704,29.1520168835031,0.158784719225683));
#12838=CARTESIAN_POINT('Ctrl Pts',(37.5424734719262,30.999648896553,0.0529282397418953));
#12839=CARTESIAN_POINT('Ctrl Pts',(38.086534003335,31.635987203375,0.));
#12840=CARTESIAN_POINT('Ctrl Pts',(38.086534003335,31.635987203375,0.));
#12841=CARTESIAN_POINT('Ctrl Pts',(38.0249211977032,31.5780862952513,1.31416644246444E-16));
#12842=CARTESIAN_POINT('Ctrl Pts',(37.9666795658435,31.5170348772935,-1.65265760471522E-15));
#12843=CARTESIAN_POINT('Ctrl Pts',(37.9118059968576,31.4532177469288,-1.0547118733939E-15));
#12844=CARTESIAN_POINT('Ctrl Pts',(37.8554797506553,31.3877111749439,-4.40936624208665E-16));
#12845=CARTESIAN_POINT('Ctrl Pts',(37.8027018184566,31.3192900860968,7.34498374270318E-16));
#12846=CARTESIAN_POINT('Ctrl Pts',(37.7534943850504,31.248322100481,1.38777878078145E-15));
#12847=CARTESIAN_POINT('Ctrl Pts',(37.7025927286682,31.1749106711927,2.063551778308E-15));
#12848=CARTESIAN_POINT('Ctrl Pts',(37.6555110871616,31.0987734236319,-2.49260826547319E-16));
#12849=CARTESIAN_POINT('Ctrl Pts',(37.6123089458347,31.0202732787551,-1.66533453693773E-16));
#12850=CARTESIAN_POINT('Ctrl Pts',(37.5934080090042,30.9859294653715,-1.30340228070347E-16));
#12851=CARTESIAN_POINT('Ctrl Pts',(37.5752501267739,30.9511328723943,9.4717807460593E-16));
#12852=CARTESIAN_POINT('Ctrl Pts',(37.5578427256908,30.9159118020698,9.43689570931383E-16));
#12853=CARTESIAN_POINT('Ctrl Pts',(37.5483345257469,30.8966734920379,9.4178409461791E-16));
#12854=CARTESIAN_POINT('Ctrl Pts',(37.5390502604861,30.877308518724,3.47271198083739E-15));
#12855=CARTESIAN_POINT('Ctrl Pts',(37.529991343845,30.8578213657365,3.66373598126302E-15));
#12856=CARTESIAN_POINT('Ctrl Pts',(37.521341388929,30.8392139536738,3.84613626785524E-15));
#12857=CARTESIAN_POINT('Ctrl Pts',(37.5128944050193,30.8204891453965,3.43625081085264E-15));
#12858=CARTESIAN_POINT('Ctrl Pts',(37.5046657230374,30.8016836240999,3.49720252756924E-15));
#12859=CARTESIAN_POINT('Ctrl Pts',(37.4681048541193,30.7181287849921,3.76801718903391E-15));
#12860=CARTESIAN_POINT('Ctrl Pts',(37.4358042063432,30.6328904850717,1.83819694350877E-15));
#12861=CARTESIAN_POINT('Ctrl Pts',(37.4077880529032,30.5463675702544,1.60982338570648E-15));
#12862=CARTESIAN_POINT('Ctrl Pts',(37.3793096171943,30.4584169787416,1.37768153591975E-15));
#12863=CARTESIAN_POINT('Ctrl Pts',(37.3552577435286,30.3691382731478,2.54125228512118E-15));
#12864=CARTESIAN_POINT('Ctrl Pts',(37.3356970343403,30.2789132420247,2.63677968348475E-15));
#12865=CARTESIAN_POINT('Ctrl Pts',(37.316474608434,30.1902485643299,2.73065502917864E-15));
#12866=CARTESIAN_POINT('Ctrl Pts',(37.3015890909228,30.1006691003133,-1.19299483480687E-15));
#12867=CARTESIAN_POINT('Ctrl Pts',(37.2911444905801,30.01051432614,-1.11022302462516E-15));
#12868=CARTESIAN_POINT('Ctrl Pts',(37.2870143326577,29.9748639955796,-1.07749217458295E-15));
#12869=CARTESIAN_POINT('Ctrl Pts',(37.2835790912838,29.9391235236307,1.64690140981544E-15));
#12870=CARTESIAN_POINT('Ctrl Pts',(37.2808472267473,29.9033133666839,1.9151347174784E-15));
#12871=CARTESIAN_POINT('Ctrl Pts',(37.279230311654,29.8821183248032,2.07389459664214E-15));
#12872=CARTESIAN_POINT('Ctrl Pts',(37.2778598211019,29.8608988672751,1.32362561983342E-15));
#12873=CARTESIAN_POINT('Ctrl Pts',(37.2767377116473,29.8396592126925,1.47104550762833E-15));
#12874=CARTESIAN_POINT('Ctrl Pts',(37.2759907997416,29.8255214199689,1.56917289519332E-15));
#12875=CARTESIAN_POINT('Ctrl Pts',(37.2753540163908,29.8113746821749,-3.79292133871148E-15));
#12876=CARTESIAN_POINT('Ctrl Pts',(37.2748282896725,29.7972347995588,-3.58046925441613E-15));
#12877=CARTESIAN_POINT('Ctrl Pts',(37.271289501429,29.7020559763699,-2.15040509360744E-15));
#12878=CARTESIAN_POINT('Ctrl Pts',(37.2727694520664,29.6070261797158,5.94361540829616E-15));
#12879=CARTESIAN_POINT('Ctrl Pts',(37.2793267916415,29.5125441300592,5.02375918642883E-15));
#12880=CARTESIAN_POINT('Ctrl Pts',(37.2858616393742,29.4183861562479,4.10705809491485E-15));
#12881=CARTESIAN_POINT('Ctrl Pts',(37.2974387453601,29.3247712248665,1.93403274150591E-15));
#12882=CARTESIAN_POINT('Ctrl Pts',(37.3141641558389,29.2320760646995,2.44249065417534E-15));
#12883=CARTESIAN_POINT('Ctrl Pts',(37.3161010199708,29.2213416237625,2.50137195307623E-15));
#12884=CARTESIAN_POINT('Ctrl Pts',(37.3181069820462,29.2106195069702,5.84958917054875E-15));
#12885=CARTESIAN_POINT('Ctrl Pts',(37.3201822519865,29.199910292911,5.99520433297585E-15));
#12886=CARTESIAN_POINT('Ctrl Pts',(37.3377271674815,29.109371586578,7.22834140910308E-15));
#12887=CARTESIAN_POINT('Ctrl Pts',(37.3602214707246,29.0197547944519,4.68527759423326E-15));
#12888=CARTESIAN_POINT('Ctrl Pts',(37.3873898680817,28.9312978449583,4.08006961549745E-15));
#12889=CARTESIAN_POINT('Ctrl Pts',(37.3981381405763,28.8963027959425,3.84063921458696E-15));
#12890=CARTESIAN_POINT('Ctrl Pts',(37.4096185476567,28.8614893276667,2.28153659614193E-15));
#12891=CARTESIAN_POINT('Ctrl Pts',(37.4218162374507,28.8268725147577,2.41473507855972E-15));
#12892=CARTESIAN_POINT('Ctrl Pts',(37.427770307641,28.8099749761822,2.4797533834154E-15));
#12893=CARTESIAN_POINT('Ctrl Pts',(37.4338953041512,28.7931242992959,-2.54918434296526E-16));
#12894=CARTESIAN_POINT('Ctrl Pts',(37.4401896006146,28.7763222655356,-3.60822483003176E-16));
#12895=CARTESIAN_POINT('Ctrl Pts',(37.4454344715524,28.7623215747388,-4.49069528641816E-16));
#12896=CARTESIAN_POINT('Ctrl Pts',(37.4507940003222,28.7483624662939,-9.55594185352511E-17));
#12897=CARTESIAN_POINT('Ctrl Pts',(37.4562649710241,28.7344505244132,0.));
#12898=CARTESIAN_POINT('Ctrl Pts',(37.4904895705801,28.6474219757606,5.97788401973891E-16));
#12899=CARTESIAN_POINT('Ctrl Pts',(37.5290926132927,28.5621815406575,-1.01907588556041E-15));
#12900=CARTESIAN_POINT('Ctrl Pts',(37.5717416121145,28.4789610925679,-8.04911692853238E-16));
#12901=CARTESIAN_POINT('Ctrl Pts',(37.6159708476505,28.392657148709,-5.82812258299535E-16));
#12902=CARTESIAN_POINT('Ctrl Pts',(37.6645515459853,28.3085249287516,3.03185407248741E-15));
#12903=CARTESIAN_POINT('Ctrl Pts',(37.7171688370768,28.2268265748556,2.91433543964104E-15));
#12904=CARTESIAN_POINT('Ctrl Pts',(37.7703637738187,28.1442313162008,2.79552665814381E-15));
#12905=CARTESIAN_POINT('Ctrl Pts',(37.82768483747,28.0641228383192,1.3259987157817E-15));
#12906=CARTESIAN_POINT('Ctrl Pts',(37.8888582908095,27.9867873691188,1.52655665885959E-15));
#12907=CARTESIAN_POINT('Ctrl Pts',(37.9126752729538,27.9566779443845,1.60464093706217E-15));
#12908=CARTESIAN_POINT('Ctrl Pts',(37.9370767223879,27.9269890875379,2.09229451977724E-15));
#12909=CARTESIAN_POINT('Ctrl Pts',(37.9620483501692,27.8977387304677,2.35922392732846E-15));
#12910=CARTESIAN_POINT('Ctrl Pts',(37.9820324481196,27.8743304846818,2.57284009496863E-15));
#12911=CARTESIAN_POINT('Ctrl Pts',(38.0023817288993,27.8512030803908,8.27742804330915E-16));
#12912=CARTESIAN_POINT('Ctrl Pts',(38.0230893052639,27.8283660499001,9.85322934354826E-16));
#12913=CARTESIAN_POINT('Ctrl Pts',(38.0346401981847,27.8156273261991,1.07322270477195E-15));
#12914=CARTESIAN_POINT('Ctrl Pts',(38.0462975091725,27.8029846107706,4.1054544629886E-15));
#12915=CARTESIAN_POINT('Ctrl Pts',(38.0580549739782,27.7904443387168,4.08006961549745E-15));
#12916=CARTESIAN_POINT('Ctrl Pts',(38.1271103604421,27.7167912725716,3.93097621119732E-15));
#12917=CARTESIAN_POINT('Ctrl Pts',(38.1996663368624,27.6466156377666,4.44679118004536E-17));
#12918=CARTESIAN_POINT('Ctrl Pts',(38.2754109622693,27.5802062876346,1.93595139919012E-15));
#12919=CARTESIAN_POINT('Ctrl Pts',(38.3396619945932,27.5238739831441,3.54041859452371E-15));
#12920=CARTESIAN_POINT('Ctrl Pts',(38.4062084577275,27.4702516590102,4.21609339266478E-15));
#12921=CARTESIAN_POINT('Ctrl Pts',(38.474884814511,27.4195305445025,4.49640324973188E-15));
#12922=CARTESIAN_POINT('Ctrl Pts',(38.4975730150005,27.4027741108636,4.58900755395234E-15));
#12923=CARTESIAN_POINT('Ctrl Pts',(38.5204938400916,27.3863344534043,7.30713928788027E-15));
#12924=CARTESIAN_POINT('Ctrl Pts',(38.5436417920506,27.370218907676,7.78543896018391E-15));
#12925=CARTESIAN_POINT('Ctrl Pts',(38.5602378257786,27.358664790883,8.12835817427495E-15));
#12926=CARTESIAN_POINT('Ctrl Pts',(38.5769515782062,27.3472767508646,7.01631171217938E-15));
#12927=CARTESIAN_POINT('Ctrl Pts',(38.5937664597273,27.3360669813717,6.82093270754081E-15));
#12928=CARTESIAN_POINT('Ctrl Pts',(38.6801203856795,27.27849847555,5.81755102578388E-15));
#12929=CARTESIAN_POINT('Ctrl Pts',(38.7692237014379,27.2255682326337,2.2208055584883E-15));
#12930=CARTESIAN_POINT('Ctrl Pts',(38.8607678601949,27.1775977188098,1.64104840827406E-15));
#12931=CARTESIAN_POINT('Ctrl Pts',(38.9523120189519,27.1296272049858,1.06129125805982E-15));
#12932=CARTESIAN_POINT('Ctrl Pts',(39.0462976660425,27.0866155095581,-3.08948526585221E-15));
#12933=CARTESIAN_POINT('Ctrl Pts',(39.1424542982338,27.0489248453569,-3.74960479332387E-15));
#12934=CARTESIAN_POINT('Ctrl Pts',(39.1630222702032,27.0408627854955,-3.85678960606204E-15));
#12935=CARTESIAN_POINT('Ctrl Pts',(39.1836896904282,27.033044358642,-2.30566390043011E-15));
#12936=CARTESIAN_POINT('Ctrl Pts',(39.2044526546617,27.0254683880106,-2.24820162486594E-15));
#12937=CARTESIAN_POINT('Ctrl Pts',(37.4857777211518,30.0014129073083,9.11258330249198));
#12938=CARTESIAN_POINT('Ctrl Pts',(37.4840983822515,30.328550656152,9.09196520028264));
#12939=CARTESIAN_POINT('Ctrl Pts',(37.5433553669445,30.6551052822669,9.0713470980733));
#12940=CARTESIAN_POINT('Ctrl Pts',(37.6663751405423,30.9555493849948,9.05072899586396));
#12941=CARTESIAN_POINT('Ctrl Pts',(37.9821762750923,31.7268122944889,8.99780075612207));
#12942=CARTESIAN_POINT('Ctrl Pts',(38.7181665551061,32.3260099807071,8.94487251638018));
#12943=CARTESIAN_POINT('Ctrl Pts',(39.5374365897001,32.4788843609168,8.89194427663828));
#12944=CARTESIAN_POINT('Ctrl Pts',(40.3567066242941,32.6317587411266,8.83901603689639));
#12945=CARTESIAN_POINT('Ctrl Pts',(41.2592564134683,32.3383098153278,8.78608779715449));
#12946=CARTESIAN_POINT('Ctrl Pts',(41.8319592185383,31.7328515349137,8.73315955741259));
#12947=CARTESIAN_POINT('Ctrl Pts',(42.4046620236084,31.1273932544996,8.6802313176707));
#12948=CARTESIAN_POINT('Ctrl Pts',(42.6475178445743,30.20992561947,8.62730307792881));
#12949=CARTESIAN_POINT('Ctrl Pts',(42.4493574424489,29.4004168052366,8.57437483818691));
#12950=CARTESIAN_POINT('Ctrl Pts',(42.2511970403234,28.5909079910033,8.52144659844502));
#12951=CARTESIAN_POINT('Ctrl Pts',(41.6120204151065,27.8893579975662,8.46851835870312));
#12952=CARTESIAN_POINT('Ctrl Pts',(40.8244073873341,27.6168930641665,8.41559011896123));
#12953=CARTESIAN_POINT('Ctrl Pts',(40.0367943595617,27.3444281307668,8.36266187921933));
#12954=CARTESIAN_POINT('Ctrl Pts',(39.1007449292338,27.5010482574046,8.30973363947744));
#12955=CARTESIAN_POINT('Ctrl Pts',(38.444726990219,28.0150631146238,8.25680539973555));
#12956=CARTESIAN_POINT('Ctrl Pts',(37.8488744204282,28.4819361303902,8.20873136732103));
#12957=CARTESIAN_POINT('Ctrl Pts',(37.484043710445,29.2436545399986,8.1606573349065));
#12958=CARTESIAN_POINT('Ctrl Pts',(37.4791973108607,30.0013273487219,8.11258330249198));
#12959=CARTESIAN_POINT('Origin',(40.,-30.,5.));
#12960=CARTESIAN_POINT('Origin',(-40.,-30.,5.));
#12961=CARTESIAN_POINT('Origin',(-40.,30.,5.));
#12962=CARTESIAN_POINT('Origin',(40.,30.,5.));
#12963=CARTESIAN_POINT('Origin',(60.,50.,0.));
#12964=CARTESIAN_POINT('',(60.,50.,0.));
#12965=CARTESIAN_POINT('',(-60.,50.,0.));
#12966=CARTESIAN_POINT('',(60.,50.,0.));
#12967=CARTESIAN_POINT('',(-60.,50.,0.));
#12968=CARTESIAN_POINT('',(60.,50.,0.));
#12969=CARTESIAN_POINT('Origin',(60.,-50.,0.));
#12970=CARTESIAN_POINT('',(60.,-50.,0.));
#12971=CARTESIAN_POINT('',(60.,-50.,0.));
#12972=CARTESIAN_POINT('',(60.,-50.,0.));
#12973=CARTESIAN_POINT('Origin',(-60.,-50.,0.));
#12974=CARTESIAN_POINT('',(-60.,-50.,0.));
#12975=CARTESIAN_POINT('',(-60.,-50.,0.));
#12976=CARTESIAN_POINT('',(-60.,-50.,0.));
#12977=CARTESIAN_POINT('Origin',(-60.,50.,0.));
#12978=CARTESIAN_POINT('',(-60.,50.,0.));
#12979=CARTESIAN_POINT('Origin',(0.,0.,0.));
#12980=CARTESIAN_POINT('',(0.,0.,0.));
#12981=CARTESIAN_POINT('Origin',(60.,1.,240.));
#12982=CARTESIAN_POINT('',(60.,1.,240.));
#12983=CARTESIAN_POINT('',(-60.,1.,240.));
#12984=CARTESIAN_POINT('',(60.,1.,240.));
#12985=CARTESIAN_POINT('',(-60.,1.,280.));
#12986=CARTESIAN_POINT('',(-60.,1.,240.));
#12987=CARTESIAN_POINT('',(60.,1.,280.));
#12988=CARTESIAN_POINT('',(60.,1.,280.));
#12989=CARTESIAN_POINT('',(60.,1.,240.));
#12990=CARTESIAN_POINT('Origin',(60.,-1.,240.));
#12991=CARTESIAN_POINT('',(60.,-1.,240.));
#12992=CARTESIAN_POINT('',(60.,-1.,240.));
#12993=CARTESIAN_POINT('',(60.,-1.,280.));
#12994=CARTESIAN_POINT('',(60.,-1.,280.));
#12995=CARTESIAN_POINT('',(60.,-1.,240.));
#12996=CARTESIAN_POINT('Origin',(-60.,-1.,240.));
#12997=CARTESIAN_POINT('',(-60.,-1.,240.));
#12998=CARTESIAN_POINT('',(-60.,-1.,240.));
#12999=CARTESIAN_POINT('',(-60.,-1.,280.));
#13000=CARTESIAN_POINT('',(-60.,-1.,280.));
#13001=CARTESIAN_POINT('',(-60.,-1.,240.));
#13002=CARTESIAN_POINT('Origin',(-60.,1.,240.));
#13003=CARTESIAN_POINT('',(-60.,1.,240.));
#13004=CARTESIAN_POINT('',(-60.,1.,280.));
#13005=CARTESIAN_POINT('Origin',(0.,0.,280.));
#13006=CARTESIAN_POINT('Origin',(0.,0.,240.));
#13007=CARTESIAN_POINT('',(0.,0.,0.));
#13008=CARTESIAN_POINT('Origin',(0.,0.,0.));
#13009=CARTESIAN_POINT('',(-8.,-9.79717439317883E-16,16.));
#13010=CARTESIAN_POINT('Origin',(0.,0.,16.));
#13011=CARTESIAN_POINT('',(-8.,-9.79717439317883E-16,0.));
#13012=CARTESIAN_POINT('',(-8.,-9.79717439317883E-16,0.));
#13013=CARTESIAN_POINT('Origin',(0.,0.,0.));
#13014=CARTESIAN_POINT('Origin',(0.,0.,0.));
#13015=CARTESIAN_POINT('',(-15.,-1.83697019872103E-15,16.));
#13016=CARTESIAN_POINT('Origin',(0.,0.,16.));
#13017=CARTESIAN_POINT('',(-15.,-1.83697019872103E-15,0.));
#13018=CARTESIAN_POINT('',(-15.,-1.83697019872103E-15,0.));
#13019=CARTESIAN_POINT('Origin',(0.,0.,0.));
#13020=CARTESIAN_POINT('Origin',(0.,0.,16.));
#13021=CARTESIAN_POINT('Origin',(0.,0.,0.));
#13022=CARTESIAN_POINT('',(0.,0.,0.));
#13023=CARTESIAN_POINT('Origin',(0.,0.,0.));
#13024=CARTESIAN_POINT('',(-6.,-7.34788079488412E-16,16.));
#13025=CARTESIAN_POINT('Origin',(0.,0.,16.));
#13026=CARTESIAN_POINT('',(-6.,-7.34788079488412E-16,0.));
#13027=CARTESIAN_POINT('',(-6.,-7.34788079488412E-16,0.));
#13028=CARTESIAN_POINT('Origin',(0.,0.,0.));
#13029=CARTESIAN_POINT('Origin',(0.,0.,0.));
#13030=CARTESIAN_POINT('',(-8.,-9.79717439317883E-16,16.));
#13031=CARTESIAN_POINT('Origin',(0.,0.,16.));
#13032=CARTESIAN_POINT('',(-8.,-9.79717439317883E-16,0.));
#13033=CARTESIAN_POINT('',(-8.,-9.79717439317883E-16,0.));
#13034=CARTESIAN_POINT('Origin',(0.,0.,0.));
#13035=CARTESIAN_POINT('Origin',(0.,0.,16.));
#13036=CARTESIAN_POINT('Origin',(0.,0.,0.));
#13037=CARTESIAN_POINT('',(0.,0.,0.));
#13038=CARTESIAN_POINT('Origin',(0.,0.,104.5));
#13039=CARTESIAN_POINT('',(-5.,-6.12323399573677E-16,104.));
#13040=CARTESIAN_POINT('Origin',(0.,0.,104.));
#13041=CARTESIAN_POINT('',(-5.,-6.12323399573677E-16,105.));
#13042=CARTESIAN_POINT('',(-5.,-6.12323399573677E-16,104.5));
#13043=CARTESIAN_POINT('Origin',(0.,0.,105.));
#13044=CARTESIAN_POINT('Origin',(9.,0.,104.));
#13045=CARTESIAN_POINT('',(-6.,7.34788079488412E-16,104.));
#13046=CARTESIAN_POINT('Origin',(0.,0.,104.));
#13047=CARTESIAN_POINT('Origin',(5.,0.,105.));
#13048=CARTESIAN_POINT('',(-6.,-7.34788079488412E-16,105.));
#13049=CARTESIAN_POINT('Origin',(0.,0.,105.));
#13050=CARTESIAN_POINT('Origin',(0.,0.,0.));
#13051=CARTESIAN_POINT('',(-6.,-7.34788079488412E-16,106.));
#13052=CARTESIAN_POINT('Origin',(0.,0.,106.));
#13053=CARTESIAN_POINT('',(-6.,-7.34788079488412E-16,0.));
#13054=CARTESIAN_POINT('Origin',(0.,0.,0.));
#13055=CARTESIAN_POINT('',(-9.,-1.10218211923262E-15,0.));
#13056=CARTESIAN_POINT('Origin',(0.,0.,0.));
#13057=CARTESIAN_POINT('',(-6.,-7.34788079488412E-16,0.));
#13058=CARTESIAN_POINT('Origin',(0.,0.,0.));
#13059=CARTESIAN_POINT('Origin',(0.,0.,-4.));
#13060=CARTESIAN_POINT('',(-9.,-1.10218211923262E-15,-4.));
#13061=CARTESIAN_POINT('',(-9.,-1.10218211923262E-15,-4.));
#13062=CARTESIAN_POINT('Origin',(0.,0.,-4.));
#13063=CARTESIAN_POINT('Origin',(0.,0.,-4.));
#13064=CARTESIAN_POINT('Origin',(0.,0.,0.));
#13065=CARTESIAN_POINT('',(-6.,-7.34788079488412E-16,0.));
#13066=CARTESIAN_POINT('Origin',(0.,0.,106.));
#13067=CARTESIAN_POINT('',(0.,0.,0.));
#13068=CARTESIAN_POINT('Origin',(-1.,0.,1.));
#13069=CARTESIAN_POINT('',(-1.,4.89897948556636,0.));
#13070=CARTESIAN_POINT('',(-1.,4.89897948556636,1.));
#13071=CARTESIAN_POINT('',(-1.,4.89897948556636,0.));
#13072=CARTESIAN_POINT('',(-1.,8.94427190999916,0.));
#13073=CARTESIAN_POINT('',(-1.,0.,0.));
#13074=CARTESIAN_POINT('',(-1.,8.94427190999916,1.));
#13075=CARTESIAN_POINT('',(-1.,8.94427190999916,0.));
#13076=CARTESIAN_POINT('',(-1.,0.,1.));
#13077=CARTESIAN_POINT('Origin',(1.,18.,1.));
#13078=CARTESIAN_POINT('',(1.,4.89897948556636,1.));
#13079=CARTESIAN_POINT('',(1.,4.89897948556636,0.));
#13080=CARTESIAN_POINT('',(1.,4.89897948556636,0.));
#13081=CARTESIAN_POINT('',(1.,8.94427190999916,1.));
#13082=CARTESIAN_POINT('',(1.,9.,1.));
#13083=CARTESIAN_POINT('',(1.,8.94427190999916,0.));
#13084=CARTESIAN_POINT('',(1.,8.94427190999916,0.));
#13085=CARTESIAN_POINT('',(1.,9.,0.));
#13086=CARTESIAN_POINT('Origin',(0.,0.,0.));
#13087=CARTESIAN_POINT('Origin',(0.,0.,0.));
#13088=CARTESIAN_POINT('Origin',(0.,0.,0.));
#13089=CARTESIAN_POINT('Origin',(0.,0.,0.));
#13090=CARTESIAN_POINT('Origin',(0.,0.,1.));
#13091=CARTESIAN_POINT('Origin',(0.,0.,0.));
#13092=CARTESIAN_POINT('Origin',(0.,0.,1.));
#13093=CARTESIAN_POINT('Origin',(0.,0.,1.));
#13094=CARTESIAN_POINT('',(0.,0.,0.));
#13095=CARTESIAN_POINT('Origin',(0.,0.,0.));
#13096=CARTESIAN_POINT('',(-6.,-7.34788079488412E-16,33.));
#13097=CARTESIAN_POINT('Origin',(0.,0.,33.));
#13098=CARTESIAN_POINT('',(-6.,-7.34788079488412E-16,0.));
#13099=CARTESIAN_POINT('',(-6.,-7.34788079488412E-16,0.));
#13100=CARTESIAN_POINT('Origin',(0.,0.,0.));
#13101=CARTESIAN_POINT('Origin',(0.,0.,0.));
#13102=CARTESIAN_POINT('',(-10.,-1.22464679914735E-15,33.));
#13103=CARTESIAN_POINT('Origin',(0.,0.,33.));
#13104=CARTESIAN_POINT('',(-10.,-1.22464679914735E-15,0.));
#13105=CARTESIAN_POINT('',(-10.,-1.22464679914735E-15,0.));
#13106=CARTESIAN_POINT('Origin',(0.,0.,0.));
#13107=CARTESIAN_POINT('Origin',(0.,0.,33.));
#13108=CARTESIAN_POINT('Origin',(0.,0.,0.));
#13109=CARTESIAN_POINT('',(0.,0.,0.));
#13110=CARTESIAN_POINT('Origin',(0.,0.,0.));
#13111=CARTESIAN_POINT('',(-6.,-7.34788079488412E-16,1.));
#13112=CARTESIAN_POINT('Origin',(0.,0.,1.));
#13113=CARTESIAN_POINT('',(-6.,-7.34788079488412E-16,0.));
#13114=CARTESIAN_POINT('',(-6.,-7.34788079488412E-16,0.));
#13115=CARTESIAN_POINT('Origin',(0.,0.,0.));
#13116=CARTESIAN_POINT('Origin',(0.,0.,0.));
#13117=CARTESIAN_POINT('',(-11.,-1.34711147906209E-15,1.));
#13118=CARTESIAN_POINT('Origin',(0.,0.,1.));
#13119=CARTESIAN_POINT('',(-11.,-1.34711147906209E-15,0.));
#13120=CARTESIAN_POINT('',(-11.,-1.34711147906209E-15,0.));
#13121=CARTESIAN_POINT('Origin',(0.,0.,0.));
#13122=CARTESIAN_POINT('Origin',(0.,0.,1.));
#13123=CARTESIAN_POINT('Origin',(0.,0.,0.));
#13124=CARTESIAN_POINT('',(0.,0.,0.));
#13125=CARTESIAN_POINT('Origin',(0.,0.,0.));
#13126=CARTESIAN_POINT('',(-6.,-7.34788079488412E-16,2.));
#13127=CARTESIAN_POINT('Origin',(0.,0.,2.));
#13128=CARTESIAN_POINT('',(-6.,-7.34788079488412E-16,0.));
#13129=CARTESIAN_POINT('',(-6.,-7.34788079488412E-16,0.));
#13130=CARTESIAN_POINT('Origin',(0.,0.,0.));
#13131=CARTESIAN_POINT('Origin',(0.,0.,0.));
#13132=CARTESIAN_POINT('',(-11.,-1.34711147906209E-15,2.));
#13133=CARTESIAN_POINT('Origin',(0.,0.,2.));
#13134=CARTESIAN_POINT('',(-11.,-1.34711147906209E-15,0.));
#13135=CARTESIAN_POINT('',(-11.,-1.34711147906209E-15,0.));
#13136=CARTESIAN_POINT('Origin',(0.,0.,0.));
#13137=CARTESIAN_POINT('Origin',(0.,0.,2.));
#13138=CARTESIAN_POINT('Origin',(0.,0.,0.));
#13139=CARTESIAN_POINT('',(-180.,0.,20.));
#13140=CARTESIAN_POINT('',(-200.,0.,260.));
#13141=CARTESIAN_POINT('',(180.,0.,20.));
#13142=CARTESIAN_POINT('',(-180.,0.,8.));
#13143=CARTESIAN_POINT('',(-180.,0.,0.));
#13144=CARTESIAN_POINT('',(-204.,0.,260.));
#13145=CARTESIAN_POINT('',(-155.,0.,185.));
#13146=CARTESIAN_POINT('',(-45.1783692539714,-46.,-8.10817877848355E-15));
#13147=CARTESIAN_POINT('',(-45.1783692539714,1.58618070410479E-14,190.));
#13148=CARTESIAN_POINT('',(-45.1783692539714,-41.,-7.80201707869671E-15));
#13149=CARTESIAN_POINT('',(-75.1783692539714,-8.,295.));
#13150=CARTESIAN_POINT('',(-75.1783692539714,-8.,295.));
#13151=CARTESIAN_POINT('',(-75.1783692539714,-42.,295.));
#13152=CARTESIAN_POINT('',(-75.1783692539714,-9.00000000000003,295.));
#13153=CARTESIAN_POINT('',(-75.1783692539714,-52.,295.));
#13154=CARTESIAN_POINT('',(-75.1783692539714,-52.,295.));
#13155=CARTESIAN_POINT('',(-75.1783692539714,52.,295.));
#13156=CARTESIAN_POINT('',(180.,0.,8.));
#13157=CARTESIAN_POINT('',(180.,0.,0.));
#13158=CARTESIAN_POINT('',(200.,0.,260.));
#13159=CARTESIAN_POINT('',(155.,0.,185.));
#13160=CARTESIAN_POINT('',(-45.1783692539714,46.,3.30523332855993E-14));
#13161=CARTESIAN_POINT('',(-45.1783692539714,7.90160284659012E-15,320.));
#13162=CARTESIAN_POINT('',(-45.1783692539714,41.,3.27461715858125E-14));
#13163=CARTESIAN_POINT('',(-75.1783692539714,8.99999999999997,295.));
#13164=CARTESIAN_POINT('',(-75.1783692539714,7.99999999999997,295.));
#13165=CARTESIAN_POINT('',(-75.1783692539714,50.,295.));
#13166=CARTESIAN_POINT('',(-15.1783692539714,-8.,295.));
#13167=CARTESIAN_POINT('',(-15.1783692539714,-8.,295.));
#13168=CARTESIAN_POINT('',(-15.1783692539714,-52.,295.));
#13169=CARTESIAN_POINT('',(-15.1783692539714,52.,295.));
#13170=CARTESIAN_POINT('',(-15.1783692539714,-42.,295.));
#13171=CARTESIAN_POINT('',(-15.1783692539714,8.99999999999997,295.));
#13172=CARTESIAN_POINT('',(-15.1783692539714,-9.00000000000003,295.));
#13173=CARTESIAN_POINT('',(-15.1783692539714,7.99999999999997,295.));
#13174=CARTESIAN_POINT('',(-15.1783692539714,-52.,295.));
#13175=CARTESIAN_POINT('',(-15.1783692539714,50.,295.));
#13176=CARTESIAN_POINT('',(-75.1783692539714,-8.,225.));
#13177=CARTESIAN_POINT('',(-75.1783692539714,-8.,225.));
#13178=CARTESIAN_POINT('',(-75.1783692539714,-52.,225.));
#13179=CARTESIAN_POINT('',(-75.1783692539714,52.,225.));
#13180=CARTESIAN_POINT('',(-75.1783692539714,-42.,225.));
#13181=CARTESIAN_POINT('',(-75.1783692539714,9.00000000000002,225.));
#13182=CARTESIAN_POINT('',(-75.1783692539714,-8.99999999999999,225.));
#13183=CARTESIAN_POINT('',(-75.1783692539714,8.00000000000001,225.));
#13184=CARTESIAN_POINT('',(-75.1783692539714,-52.,225.));
#13185=CARTESIAN_POINT('',(-75.1783692539714,50.,225.));
#13186=CARTESIAN_POINT('',(-15.1783692539714,-8.,225.));
#13187=CARTESIAN_POINT('',(-15.1783692539714,-8.,225.));
#13188=CARTESIAN_POINT('',(-15.1783692539714,-52.,225.));
#13189=CARTESIAN_POINT('',(-15.1783692539714,52.,225.));
#13190=CARTESIAN_POINT('',(-15.1783692539714,-42.,225.));
#13191=CARTESIAN_POINT('',(-15.1783692539714,9.00000000000002,225.));
#13192=CARTESIAN_POINT('',(-15.1783692539714,-8.99999999999999,225.));
#13193=CARTESIAN_POINT('',(-15.1783692539714,8.00000000000001,225.));
#13194=CARTESIAN_POINT('',(-15.1783692539714,-52.,225.));
#13195=CARTESIAN_POINT('',(-15.1783692539714,50.,225.));
#13196=UNCERTAINTY_MEASURE_WITH_UNIT(LENGTH_MEASURE(0.01),#13232,
'DISTANCE_ACCURACY_VALUE',
'Maximum model space distance between geometric entities at asserted c
onnectivities');
#13197=UNCERTAINTY_MEASURE_WITH_UNIT(LENGTH_MEASURE(0.01),#13232,
'DISTANCE_ACCURACY_VALUE',
'Maximum model space distance between geometric entities at asserted c
onnectivities');
#13198=UNCERTAINTY_MEASURE_WITH_UNIT(LENGTH_MEASURE(0.01),#13232,
'DISTANCE_ACCURACY_VALUE',
'Maximum model space distance between geometric entities at asserted c
onnectivities');
#13199=UNCERTAINTY_MEASURE_WITH_UNIT(LENGTH_MEASURE(0.01),#13232,
'DISTANCE_ACCURACY_VALUE',
'Maximum model space distance between geometric entities at asserted c
onnectivities');
#13200=UNCERTAINTY_MEASURE_WITH_UNIT(LENGTH_MEASURE(0.01),#13232,
'DISTANCE_ACCURACY_VALUE',
'Maximum model space distance between geometric entities at asserted c
onnectivities');
#13201=UNCERTAINTY_MEASURE_WITH_UNIT(LENGTH_MEASURE(0.01),#13232,
'DISTANCE_ACCURACY_VALUE',
'Maximum model space distance between geometric entities at asserted c
onnectivities');
#13202=UNCERTAINTY_MEASURE_WITH_UNIT(LENGTH_MEASURE(0.01),#13232,
'DISTANCE_ACCURACY_VALUE',
'Maximum model space distance between geometric entities at asserted c
onnectivities');
#13203=UNCERTAINTY_MEASURE_WITH_UNIT(LENGTH_MEASURE(0.01),#13232,
'DISTANCE_ACCURACY_VALUE',
'Maximum model space distance between geometric entities at asserted c
onnectivities');
#13204=UNCERTAINTY_MEASURE_WITH_UNIT(LENGTH_MEASURE(0.01),#13232,
'DISTANCE_ACCURACY_VALUE',
'Maximum model space distance between geometric entities at asserted c
onnectivities');
#13205=UNCERTAINTY_MEASURE_WITH_UNIT(LENGTH_MEASURE(0.01),#13232,
'DISTANCE_ACCURACY_VALUE',
'Maximum model space distance between geometric entities at asserted c
onnectivities');
#13206=UNCERTAINTY_MEASURE_WITH_UNIT(LENGTH_MEASURE(0.01),#13232,
'DISTANCE_ACCURACY_VALUE',
'Maximum model space distance between geometric entities at asserted c
onnectivities');
#13207=UNCERTAINTY_MEASURE_WITH_UNIT(LENGTH_MEASURE(0.01),#13232,
'DISTANCE_ACCURACY_VALUE',
'Maximum model space distance between geometric entities at asserted c
onnectivities');
#13208=UNCERTAINTY_MEASURE_WITH_UNIT(LENGTH_MEASURE(0.01),#13232,
'DISTANCE_ACCURACY_VALUE',
'Maximum model space distance between geometric entities at asserted c
onnectivities');
#13209=UNCERTAINTY_MEASURE_WITH_UNIT(LENGTH_MEASURE(0.01),#13232,
'DISTANCE_ACCURACY_VALUE',
'Maximum model space distance between geometric entities at asserted c
onnectivities');
#13210=UNCERTAINTY_MEASURE_WITH_UNIT(LENGTH_MEASURE(0.01),#13232,
'DISTANCE_ACCURACY_VALUE',
'Maximum model space distance between geometric entities at asserted c
onnectivities');
#13211=UNCERTAINTY_MEASURE_WITH_UNIT(LENGTH_MEASURE(0.01),#13232,
'DISTANCE_ACCURACY_VALUE',
'Maximum model space distance between geometric entities at asserted c
onnectivities');
#13212=UNCERTAINTY_MEASURE_WITH_UNIT(LENGTH_MEASURE(0.01),#13232,
'DISTANCE_ACCURACY_VALUE',
'Maximum model space distance between geometric entities at asserted c
onnectivities');
#13213=UNCERTAINTY_MEASURE_WITH_UNIT(LENGTH_MEASURE(0.01),#13232,
'DISTANCE_ACCURACY_VALUE',
'Maximum model space distance between geometric entities at asserted c
onnectivities');
#13214=(
GEOMETRIC_REPRESENTATION_CONTEXT(3)
GLOBAL_UNCERTAINTY_ASSIGNED_CONTEXT((#13196))
GLOBAL_UNIT_ASSIGNED_CONTEXT((#13232,#13234,#13235))
REPRESENTATION_CONTEXT('','3D')
);
#13215=(
GEOMETRIC_REPRESENTATION_CONTEXT(3)
GLOBAL_UNCERTAINTY_ASSIGNED_CONTEXT((#13197))
GLOBAL_UNIT_ASSIGNED_CONTEXT((#13232,#13234,#13235))
REPRESENTATION_CONTEXT('','3D')
);
#13216=(
GEOMETRIC_REPRESENTATION_CONTEXT(3)
GLOBAL_UNCERTAINTY_ASSIGNED_CONTEXT((#13198))
GLOBAL_UNIT_ASSIGNED_CONTEXT((#13232,#13234,#13235))
REPRESENTATION_CONTEXT('','3D')
);
#13217=(
GEOMETRIC_REPRESENTATION_CONTEXT(3)
GLOBAL_UNCERTAINTY_ASSIGNED_CONTEXT((#13199))
GLOBAL_UNIT_ASSIGNED_CONTEXT((#13232,#13234,#13235))
REPRESENTATION_CONTEXT('','3D')
);
#13218=(
GEOMETRIC_REPRESENTATION_CONTEXT(3)
GLOBAL_UNCERTAINTY_ASSIGNED_CONTEXT((#13200))
GLOBAL_UNIT_ASSIGNED_CONTEXT((#13232,#13234,#13235))
REPRESENTATION_CONTEXT('','3D')
);
#13219=(
GEOMETRIC_REPRESENTATION_CONTEXT(3)
GLOBAL_UNCERTAINTY_ASSIGNED_CONTEXT((#13201))
GLOBAL_UNIT_ASSIGNED_CONTEXT((#13232,#13234,#13235))
REPRESENTATION_CONTEXT('','3D')
);
#13220=(
GEOMETRIC_REPRESENTATION_CONTEXT(3)
GLOBAL_UNCERTAINTY_ASSIGNED_CONTEXT((#13202))
GLOBAL_UNIT_ASSIGNED_CONTEXT((#13232,#13234,#13235))
REPRESENTATION_CONTEXT('','3D')
);
#13221=(
GEOMETRIC_REPRESENTATION_CONTEXT(3)
GLOBAL_UNCERTAINTY_ASSIGNED_CONTEXT((#13203))
GLOBAL_UNIT_ASSIGNED_CONTEXT((#13232,#13234,#13235))
REPRESENTATION_CONTEXT('','3D')
);
#13222=(
GEOMETRIC_REPRESENTATION_CONTEXT(3)
GLOBAL_UNCERTAINTY_ASSIGNED_CONTEXT((#13204))
GLOBAL_UNIT_ASSIGNED_CONTEXT((#13232,#13234,#13235))
REPRESENTATION_CONTEXT('','3D')
);
#13223=(
GEOMETRIC_REPRESENTATION_CONTEXT(3)
GLOBAL_UNCERTAINTY_ASSIGNED_CONTEXT((#13205))
GLOBAL_UNIT_ASSIGNED_CONTEXT((#13232,#13234,#13235))
REPRESENTATION_CONTEXT('','3D')
);
#13224=(
GEOMETRIC_REPRESENTATION_CONTEXT(3)
GLOBAL_UNCERTAINTY_ASSIGNED_CONTEXT((#13206))
GLOBAL_UNIT_ASSIGNED_CONTEXT((#13232,#13234,#13235))
REPRESENTATION_CONTEXT('','3D')
);
#13225=(
GEOMETRIC_REPRESENTATION_CONTEXT(3)
GLOBAL_UNCERTAINTY_ASSIGNED_CONTEXT((#13207))
GLOBAL_UNIT_ASSIGNED_CONTEXT((#13232,#13234,#13235))
REPRESENTATION_CONTEXT('','3D')
);
#13226=(
GEOMETRIC_REPRESENTATION_CONTEXT(3)
GLOBAL_UNCERTAINTY_ASSIGNED_CONTEXT((#13208))
GLOBAL_UNIT_ASSIGNED_CONTEXT((#13232,#13234,#13235))
REPRESENTATION_CONTEXT('','3D')
);
#13227=(
GEOMETRIC_REPRESENTATION_CONTEXT(3)
GLOBAL_UNCERTAINTY_ASSIGNED_CONTEXT((#13209))
GLOBAL_UNIT_ASSIGNED_CONTEXT((#13232,#13234,#13235))
REPRESENTATION_CONTEXT('','3D')
);
#13228=(
GEOMETRIC_REPRESENTATION_CONTEXT(3)
GLOBAL_UNCERTAINTY_ASSIGNED_CONTEXT((#13210))
GLOBAL_UNIT_ASSIGNED_CONTEXT((#13232,#13234,#13235))
REPRESENTATION_CONTEXT('','3D')
);
#13229=(
GEOMETRIC_REPRESENTATION_CONTEXT(3)
GLOBAL_UNCERTAINTY_ASSIGNED_CONTEXT((#13211))
GLOBAL_UNIT_ASSIGNED_CONTEXT((#13232,#13234,#13235))
REPRESENTATION_CONTEXT('','3D')
);
#13230=(
GEOMETRIC_REPRESENTATION_CONTEXT(3)
GLOBAL_UNCERTAINTY_ASSIGNED_CONTEXT((#13212))
GLOBAL_UNIT_ASSIGNED_CONTEXT((#13232,#13234,#13235))
REPRESENTATION_CONTEXT('','3D')
);
#13231=(
GEOMETRIC_REPRESENTATION_CONTEXT(3)
GLOBAL_UNCERTAINTY_ASSIGNED_CONTEXT((#13213))
GLOBAL_UNIT_ASSIGNED_CONTEXT((#13232,#13234,#13235))
REPRESENTATION_CONTEXT('','3D')
);
#13232=(
LENGTH_UNIT()
NAMED_UNIT(*)
SI_UNIT(.MILLI.,.METRE.)
);
#13233=(
LENGTH_UNIT()
NAMED_UNIT(*)
SI_UNIT($,.METRE.)
);
#13234=(
NAMED_UNIT(*)
PLANE_ANGLE_UNIT()
SI_UNIT($,.RADIAN.)
);
#13235=(
NAMED_UNIT(*)
SI_UNIT($,.STERADIAN.)
SOLID_ANGLE_UNIT()
);
#13236=SHAPE_DEFINITION_REPRESENTATION(#13253,#13327);
#13237=SHAPE_DEFINITION_REPRESENTATION(#13254,#13328);
#13238=SHAPE_DEFINITION_REPRESENTATION(#13255,#13329);
#13239=SHAPE_DEFINITION_REPRESENTATION(#13256,#13330);
#13240=SHAPE_DEFINITION_REPRESENTATION(#13257,#13331);
#13241=SHAPE_DEFINITION_REPRESENTATION(#13258,#13332);
#13242=SHAPE_DEFINITION_REPRESENTATION(#13259,#13333);
#13243=SHAPE_DEFINITION_REPRESENTATION(#13260,#13334);
#13244=SHAPE_DEFINITION_REPRESENTATION(#13261,#13335);
#13245=SHAPE_DEFINITION_REPRESENTATION(#13262,#13336);
#13246=SHAPE_DEFINITION_REPRESENTATION(#13263,#13337);
#13247=SHAPE_DEFINITION_REPRESENTATION(#13264,#13338);
#13248=SHAPE_DEFINITION_REPRESENTATION(#13265,#13339);
#13249=SHAPE_DEFINITION_REPRESENTATION(#13266,#13340);
#13250=SHAPE_DEFINITION_REPRESENTATION(#13267,#13341);
#13251=SHAPE_DEFINITION_REPRESENTATION(#13268,#13342);
#13252=SHAPE_DEFINITION_REPRESENTATION(#13269,#13343);
#13253=PRODUCT_DEFINITION_SHAPE('',$,#13345);
#13254=PRODUCT_DEFINITION_SHAPE('',$,#13346);
#13255=PRODUCT_DEFINITION_SHAPE('',$,#13347);
#13256=PRODUCT_DEFINITION_SHAPE('',$,#13348);
#13257=PRODUCT_DEFINITION_SHAPE('',$,#13349);
#13258=PRODUCT_DEFINITION_SHAPE('',$,#13350);
#13259=PRODUCT_DEFINITION_SHAPE('',$,#13351);
#13260=PRODUCT_DEFINITION_SHAPE('',$,#13352);
#13261=PRODUCT_DEFINITION_SHAPE('',$,#13353);
#13262=PRODUCT_DEFINITION_SHAPE('',$,#13354);
#13263=PRODUCT_DEFINITION_SHAPE('',$,#13355);
#13264=PRODUCT_DEFINITION_SHAPE('',$,#13356);
#13265=PRODUCT_DEFINITION_SHAPE('',$,#13357);
#13266=PRODUCT_DEFINITION_SHAPE('',$,#13358);
#13267=PRODUCT_DEFINITION_SHAPE('',$,#13359);
#13268=PRODUCT_DEFINITION_SHAPE('',$,#13360);
#13269=PRODUCT_DEFINITION_SHAPE('',$,#13361);
#13270=PRODUCT_DEFINITION_SHAPE($,$,#182);
#13271=PRODUCT_DEFINITION_SHAPE($,$,#183);
#13272=PRODUCT_DEFINITION_SHAPE($,$,#184);
#13273=PRODUCT_DEFINITION_SHAPE($,$,#185);
#13274=PRODUCT_DEFINITION_SHAPE($,$,#186);
#13275=PRODUCT_DEFINITION_SHAPE($,$,#187);
#13276=PRODUCT_DEFINITION_SHAPE($,$,#188);
#13277=PRODUCT_DEFINITION_SHAPE($,$,#189);
#13278=PRODUCT_DEFINITION_SHAPE($,$,#190);
#13279=PRODUCT_DEFINITION_SHAPE($,$,#191);
#13280=PRODUCT_DEFINITION_SHAPE($,$,#192);
#13281=PRODUCT_DEFINITION_SHAPE($,$,#193);
#13282=PRODUCT_DEFINITION_SHAPE($,$,#194);
#13283=PRODUCT_DEFINITION_SHAPE($,$,#195);
#13284=PRODUCT_DEFINITION_SHAPE($,$,#196);
#13285=PRODUCT_DEFINITION_SHAPE($,$,#197);
#13286=PRODUCT_DEFINITION_SHAPE($,$,#198);
#13287=PRODUCT_DEFINITION_SHAPE($,$,#199);
#13288=PRODUCT_DEFINITION_SHAPE($,$,#200);
#13289=PRODUCT_DEFINITION_SHAPE($,$,#201);
#13290=PRODUCT_DEFINITION_SHAPE($,$,#202);
#13291=PRODUCT_DEFINITION_SHAPE($,$,#203);
#13292=PRODUCT_DEFINITION_SHAPE($,$,#204);
#13293=PRODUCT_DEFINITION_SHAPE($,$,#205);
#13294=PRODUCT_DEFINITION_SHAPE($,$,#206);
#13295=PRODUCT_DEFINITION_SHAPE($,$,#207);
#13296=PRODUCT_DEFINITION_SHAPE($,$,#208);
#13297=PRODUCT_DEFINITION_SHAPE($,$,#209);
#13298=PRODUCT_DEFINITION_SHAPE($,$,#210);
#13299=PRODUCT_DEFINITION_SHAPE($,$,#211);
#13300=PRODUCT_DEFINITION_SHAPE($,$,#212);
#13301=PRODUCT_DEFINITION_SHAPE($,$,#213);
#13302=PRODUCT_DEFINITION_SHAPE($,$,#214);
#13303=PRODUCT_DEFINITION_SHAPE($,$,#215);
#13304=PRODUCT_DEFINITION_SHAPE($,$,#216);
#13305=PRODUCT_DEFINITION_SHAPE($,$,#217);
#13306=PRODUCT_DEFINITION_SHAPE($,$,#218);
#13307=PRODUCT_DEFINITION_SHAPE($,$,#219);
#13308=PRODUCT_DEFINITION_SHAPE($,$,#220);
#13309=PRODUCT_DEFINITION_SHAPE($,$,#221);
#13310=PRODUCT_DEFINITION_SHAPE($,$,#222);
#13311=PRODUCT_DEFINITION_SHAPE($,$,#223);
#13312=PRODUCT_DEFINITION_SHAPE($,$,#224);
#13313=PRODUCT_DEFINITION_SHAPE($,$,#225);
#13314=PRODUCT_DEFINITION_SHAPE($,$,#226);
#13315=PRODUCT_DEFINITION_SHAPE($,$,#227);
#13316=PRODUCT_DEFINITION_SHAPE($,$,#228);
#13317=PRODUCT_DEFINITION_SHAPE($,$,#229);
#13318=PRODUCT_DEFINITION_SHAPE($,$,#230);
#13319=PRODUCT_DEFINITION_SHAPE($,$,#231);
#13320=PRODUCT_DEFINITION_SHAPE($,$,#232);
#13321=PRODUCT_DEFINITION_SHAPE($,$,#233);
#13322=PRODUCT_DEFINITION_SHAPE($,$,#234);
#13323=PRODUCT_DEFINITION_SHAPE($,$,#235);
#13324=PRODUCT_DEFINITION_SHAPE($,$,#236);
#13325=PRODUCT_DEFINITION_SHAPE($,$,#237);
#13326=PRODUCT_DEFINITION_SHAPE($,$,#238);
#13327=SHAPE_REPRESENTATION('',(#4344,#4678,#4679,#4680,#4681,#4682,#4683,
#4684,#4685,#4686,#4687,#4688,#4689,#4690,#4691,#4692,#4693,#4694,#4695,
#4696,#4697,#4698,#4699,#4700,#4701,#4702,#4703,#4704,#4705,#4706,#4707,
#4708,#4709,#4710,#4711,#4712,#4713,#4714,#4715,#4716,#4717,#4718,#4719,
#4720,#4721,#4722,#4723,#4724,#4725,#4726,#4727,#4728,#4729,#4730,#4731,
#4732,#4733,#4734),#13214);
#13328=SHAPE_REPRESENTATION('',(#4345),#13215);
#13329=SHAPE_REPRESENTATION('',(#4380),#13216);
#13330=SHAPE_REPRESENTATION('',(#4415),#13217);
#13331=SHAPE_REPRESENTATION('',(#4434),#13218);
#13332=SHAPE_REPRESENTATION('',(#4453),#13219);
#13333=SHAPE_REPRESENTATION('',(#4460),#13220);
#13334=SHAPE_REPRESENTATION('',(#4467),#13221);
#13335=SHAPE_REPRESENTATION('',(#4486),#13222);
#13336=SHAPE_REPRESENTATION('',(#4597),#13223);
#13337=SHAPE_REPRESENTATION('',(#4604),#13224);
#13338=SHAPE_REPRESENTATION('',(#4613),#13225);
#13339=SHAPE_REPRESENTATION('',(#4622),#13226);
#13340=SHAPE_REPRESENTATION('',(#4640),#13227);
#13341=SHAPE_REPRESENTATION('',(#4651),#13228);
#13342=SHAPE_REPRESENTATION('',(#4660),#13229);
#13343=SHAPE_REPRESENTATION('',(#4669),#13230);
#13344=PRODUCT_DEFINITION_CONTEXT('part definition',#13397,'design');
#13345=PRODUCT_DEFINITION('MAS-650','MAS-650',#13362,#13344);
#13346=PRODUCT_DEFINITION('Bridge beam','Bridge beam',#13363,#13344);
#13347=PRODUCT_DEFINITION('Frame post','Frame post',#13364,#13344);
#13348=PRODUCT_DEFINITION('Foot plate','Foot plate',#13365,#13344);
#13349=PRODUCT_DEFINITION('Isolation pad','Isolation pad',#13366,#13344);
#13350=PRODUCT_DEFINITION('Beam end cap','Beam end cap',#13367,#13344);
#13351=PRODUCT_DEFINITION('Travel stop','Travel stop',#13368,#13344);
#13352=PRODUCT_DEFINITION('Carriage side plate','Carriage side plate',#13369,
#13344);
#13353=PRODUCT_DEFINITION('Carriage bridge plate',
'Carriage bridge plate',#13370,#13344);
#13354=PRODUCT_DEFINITION('Guide wear pad','Guide wear pad',#13371,#13344);
#13355=PRODUCT_DEFINITION('Track roller','Track roller',#13372,#13344);
#13356=PRODUCT_DEFINITION('Roller bearing bushing',
'Roller bearing bushing',#13373,#13344);
#13357=PRODUCT_DEFINITION('Roller axle','Roller axle',#13374,#13344);
#13358=PRODUCT_DEFINITION('Axle retaining ring','Axle retaining ring',#13375,
#13344);
#13359=PRODUCT_DEFINITION('Roller spacer','Roller spacer',#13376,#13344);
#13360=PRODUCT_DEFINITION('Bearing thrust washer',
'Bearing thrust washer',#13377,#13344);
#13361=PRODUCT_DEFINITION('Axle thrust washer','Axle thrust washer',#13378,
#13344);
#13362=PRODUCT_DEFINITION_FORMATION('',$,#13399);
#13363=PRODUCT_DEFINITION_FORMATION('',$,#13400);
#13364=PRODUCT_DEFINITION_FORMATION('',$,#13401);
#13365=PRODUCT_DEFINITION_FORMATION('',$,#13402);
#13366=PRODUCT_DEFINITION_FORMATION('',$,#13403);
#13367=PRODUCT_DEFINITION_FORMATION('',$,#13404);
#13368=PRODUCT_DEFINITION_FORMATION('',$,#13405);
#13369=PRODUCT_DEFINITION_FORMATION('',$,#13406);
#13370=PRODUCT_DEFINITION_FORMATION('',$,#13407);
#13371=PRODUCT_DEFINITION_FORMATION('',$,#13408);
#13372=PRODUCT_DEFINITION_FORMATION('',$,#13409);
#13373=PRODUCT_DEFINITION_FORMATION('',$,#13410);
#13374=PRODUCT_DEFINITION_FORMATION('',$,#13411);
#13375=PRODUCT_DEFINITION_FORMATION('',$,#13412);
#13376=PRODUCT_DEFINITION_FORMATION('',$,#13413);
#13377=PRODUCT_DEFINITION_FORMATION('',$,#13414);
#13378=PRODUCT_DEFINITION_FORMATION('',$,#13415);
#13379=PRODUCT_RELATED_PRODUCT_CATEGORY('MAS-650','MAS-650',(#13399));
#13380=PRODUCT_RELATED_PRODUCT_CATEGORY('Bridge beam','Bridge beam',(#13400));
#13381=PRODUCT_RELATED_PRODUCT_CATEGORY('Frame post','Frame post',(#13401));
#13382=PRODUCT_RELATED_PRODUCT_CATEGORY('Foot plate','Foot plate',(#13402));
#13383=PRODUCT_RELATED_PRODUCT_CATEGORY('Isolation pad','Isolation pad',
(#13403));
#13384=PRODUCT_RELATED_PRODUCT_CATEGORY('Beam end cap','Beam end cap',(#13404));
#13385=PRODUCT_RELATED_PRODUCT_CATEGORY('Travel stop','Travel stop',(#13405));
#13386=PRODUCT_RELATED_PRODUCT_CATEGORY('Carriage side plate',
'Carriage side plate',(#13406));
#13387=PRODUCT_RELATED_PRODUCT_CATEGORY('Carriage bridge plate',
'Carriage bridge plate',(#13407));
#13388=PRODUCT_RELATED_PRODUCT_CATEGORY('Guide wear pad',
'Guide wear pad',(#13408));
#13389=PRODUCT_RELATED_PRODUCT_CATEGORY('Track roller','Track roller',(#13409));
#13390=PRODUCT_RELATED_PRODUCT_CATEGORY('Roller bearing bushing',
'Roller bearing bushing',(#13410));
#13391=PRODUCT_RELATED_PRODUCT_CATEGORY('Roller axle','Roller axle',(#13411));
#13392=PRODUCT_RELATED_PRODUCT_CATEGORY('Axle retaining ring',
'Axle retaining ring',(#13412));
#13393=PRODUCT_RELATED_PRODUCT_CATEGORY('Roller spacer','Roller spacer',
(#13413));
#13394=PRODUCT_RELATED_PRODUCT_CATEGORY('Bearing thrust washer',
'Bearing thrust washer',(#13414));
#13395=PRODUCT_RELATED_PRODUCT_CATEGORY('Axle thrust washer',
'Axle thrust washer',(#13415));
#13396=APPLICATION_PROTOCOL_DEFINITION('international standard',
'automotive_design',2009,#13397);
#13397=APPLICATION_CONTEXT(
'Core Data for Automotive Mechanical Design Process');
#13398=PRODUCT_CONTEXT('part definition',#13397,'mechanical');
#13399=PRODUCT('MAS-650','MAS-650',
'Independent manual traversing gantry with native reusable aluminum pr
ofiles,180mm captured carriage travel, four bronze-bushed rollers, lin
ked ideal rolling motion, bonded acetal lateral guides, positive welde
d end stops and fully retained axle stacks. Editable native profile cu
t lengths220/400mm. Tool attachments viaM6 bridge-plate taps; mounted 
tool outside assembly. Welds, anchors, adhesives, fits, traction, load
/speed/structural/life ratings unassigned.',(#13398));
#13400=PRODUCT('Bridge beam','Bridge beam',
'Independent aluminum extrusion section. Whole-mm nominal die dimensio
ns; parametric saw-cut length. Select structural loading, tolerances a
nd finish for the assembly application.',(#13398));
#13401=PRODUCT('Frame post','Frame post',
'Independent aluminum extrusion section. Whole-mm nominal die dimensio
ns; parametric saw-cut length. Select structural loading, tolerances a
nd finish for the assembly application.',(#13398));
#13402=PRODUCT('Foot plate','Foot plate',$,(#13398));
#13403=PRODUCT('Isolation pad','Isolation pad',$,(#13398));
#13404=PRODUCT('Beam end cap','Beam end cap',$,(#13398));
#13405=PRODUCT('Travel stop','Travel stop','Travel stop',(#13398));
#13406=PRODUCT('Carriage side plate','Carriage side plate',$,(#13398));
#13407=PRODUCT('Carriage bridge plate','Carriage bridge plate',$,(#13398));
#13408=PRODUCT('Guide wear pad','Guide wear pad',$,(#13398));
#13409=PRODUCT('Track roller','Track roller',$,(#13398));
#13410=PRODUCT('Roller bearing bushing','Roller bearing bushing',$,(#13398));
#13411=PRODUCT('Roller axle','Roller axle','Roller axle',(#13398));
#13412=PRODUCT('Axle retaining ring','Axle retaining ring',$,(#13398));
#13413=PRODUCT('Roller spacer','Roller spacer',$,(#13398));
#13414=PRODUCT('Bearing thrust washer','Bearing thrust washer',$,(#13398));
#13415=PRODUCT('Axle thrust washer','Axle thrust washer',$,(#13398));
#13416=PRESENTATION_STYLE_ASSIGNMENT((#13430));
#13417=PRESENTATION_STYLE_ASSIGNMENT((#13431));
#13418=PRESENTATION_STYLE_ASSIGNMENT((#13432));
#13419=PRESENTATION_STYLE_ASSIGNMENT((#13433));
#13420=PRESENTATION_STYLE_ASSIGNMENT((#13434));
#13421=PRESENTATION_STYLE_ASSIGNMENT((#13435));
#13422=PRESENTATION_STYLE_ASSIGNMENT((#13436));
#13423=PRESENTATION_STYLE_ASSIGNMENT((#13437));
#13424=PRESENTATION_STYLE_ASSIGNMENT((#13438));
#13425=PRESENTATION_STYLE_ASSIGNMENT((#13439));
#13426=PRESENTATION_STYLE_ASSIGNMENT((#13440));
#13427=PRESENTATION_STYLE_ASSIGNMENT((#13441));
#13428=PRESENTATION_STYLE_ASSIGNMENT((#13442));
#13429=PRESENTATION_STYLE_ASSIGNMENT((#13443));
#13430=SURFACE_STYLE_USAGE(.BOTH.,#13444);
#13431=SURFACE_STYLE_USAGE(.BOTH.,#13445);
#13432=SURFACE_STYLE_USAGE(.BOTH.,#13446);
#13433=SURFACE_STYLE_USAGE(.BOTH.,#13447);
#13434=SURFACE_STYLE_USAGE(.BOTH.,#13448);
#13435=SURFACE_STYLE_USAGE(.BOTH.,#13449);
#13436=SURFACE_STYLE_USAGE(.BOTH.,#13450);
#13437=SURFACE_STYLE_USAGE(.BOTH.,#13451);
#13438=SURFACE_STYLE_USAGE(.BOTH.,#13452);
#13439=SURFACE_STYLE_USAGE(.BOTH.,#13453);
#13440=SURFACE_STYLE_USAGE(.BOTH.,#13454);
#13441=SURFACE_STYLE_USAGE(.BOTH.,#13455);
#13442=SURFACE_STYLE_USAGE(.BOTH.,#13456);
#13443=SURFACE_STYLE_USAGE(.BOTH.,#13457);
#13444=SURFACE_SIDE_STYLE('',(#13458));
#13445=SURFACE_SIDE_STYLE('',(#13459));
#13446=SURFACE_SIDE_STYLE('',(#13460));
#13447=SURFACE_SIDE_STYLE('',(#13461));
#13448=SURFACE_SIDE_STYLE('',(#13462));
#13449=SURFACE_SIDE_STYLE('',(#13463));
#13450=SURFACE_SIDE_STYLE('',(#13464));
#13451=SURFACE_SIDE_STYLE('',(#13465));
#13452=SURFACE_SIDE_STYLE('',(#13466));
#13453=SURFACE_SIDE_STYLE('',(#13467));
#13454=SURFACE_SIDE_STYLE('',(#13468));
#13455=SURFACE_SIDE_STYLE('',(#13469));
#13456=SURFACE_SIDE_STYLE('',(#13470));
#13457=SURFACE_SIDE_STYLE('',(#13471));
#13458=SURFACE_STYLE_FILL_AREA(#13472);
#13459=SURFACE_STYLE_FILL_AREA(#13473);
#13460=SURFACE_STYLE_FILL_AREA(#13474);
#13461=SURFACE_STYLE_FILL_AREA(#13475);
#13462=SURFACE_STYLE_FILL_AREA(#13476);
#13463=SURFACE_STYLE_FILL_AREA(#13477);
#13464=SURFACE_STYLE_FILL_AREA(#13478);
#13465=SURFACE_STYLE_FILL_AREA(#13479);
#13466=SURFACE_STYLE_FILL_AREA(#13480);
#13467=SURFACE_STYLE_FILL_AREA(#13481);
#13468=SURFACE_STYLE_FILL_AREA(#13482);
#13469=SURFACE_STYLE_FILL_AREA(#13483);
#13470=SURFACE_STYLE_FILL_AREA(#13484);
#13471=SURFACE_STYLE_FILL_AREA(#13485);
#13472=FILL_AREA_STYLE('Steel - Satin',(#13486));
#13473=FILL_AREA_STYLE('Dark blue',(#13487));
#13474=FILL_AREA_STYLE('Post gray',(#13488));
#13475=FILL_AREA_STYLE('Foot gray',(#13489));
#13476=FILL_AREA_STYLE('Charcoal',(#13490));
#13477=FILL_AREA_STYLE('Light gray',(#13491));
#13478=FILL_AREA_STYLE('Gray',(#13492));
#13479=FILL_AREA_STYLE('Light blue',(#13493));
#13480=FILL_AREA_STYLE('Wear pad gray',(#13494));
#13481=FILL_AREA_STYLE('Sky blue',(#13495));
#13482=FILL_AREA_STYLE('Bearing gray',(#13496));
#13483=FILL_AREA_STYLE('Axle gray',(#13497));
#13484=FILL_AREA_STYLE('Dark gray',(#13498));
#13485=FILL_AREA_STYLE('Bearing light gray',(#13499));
#13486=FILL_AREA_STYLE_COLOUR('Steel - Satin',#13500);
#13487=FILL_AREA_STYLE_COLOUR('Dark blue',#13501);
#13488=FILL_AREA_STYLE_COLOUR('Post gray',#13502);
#13489=FILL_AREA_STYLE_COLOUR('Foot gray',#13503);
#13490=FILL_AREA_STYLE_COLOUR('Charcoal',#13504);
#13491=FILL_AREA_STYLE_COLOUR('Light gray',#13505);
#13492=FILL_AREA_STYLE_COLOUR('Gray',#13506);
#13493=FILL_AREA_STYLE_COLOUR('Light blue',#13507);
#13494=FILL_AREA_STYLE_COLOUR('Wear pad gray',#13508);
#13495=FILL_AREA_STYLE_COLOUR('Sky blue',#13509);
#13496=FILL_AREA_STYLE_COLOUR('Bearing gray',#13510);
#13497=FILL_AREA_STYLE_COLOUR('Axle gray',#13511);
#13498=FILL_AREA_STYLE_COLOUR('Dark gray',#13512);
#13499=FILL_AREA_STYLE_COLOUR('Bearing light gray',#13513);
#13500=COLOUR_RGB('Steel - Satin',0.627450980392157,0.627450980392157,0.627450980392157);
#13501=COLOUR_RGB('Dark blue',0.0901960784313725,0.270588235294118,0.513725490196078);
#13502=COLOUR_RGB('Post gray',0.407843137254902,0.447058823529412,0.498039215686275);
#13503=COLOUR_RGB('Foot gray',0.576470588235294,0.615686274509804,0.666666666666667);
#13504=COLOUR_RGB('Charcoal',0.164705882352941,0.184313725490196,0.211764705882353);
#13505=COLOUR_RGB('Light gray',0.725490196078431,0.752941176470588,0.792156862745098);
#13506=COLOUR_RGB('Gray',0.407843137254902,0.447058823529412,0.498039215686275);
#13507=COLOUR_RGB('Light blue',0.662745098039216,0.831372549019608,0.949019607843137);
#13508=COLOUR_RGB('Wear pad gray',0.725490196078431,0.752941176470588,0.792156862745098);
#13509=COLOUR_RGB('Sky blue',0.317647058823529,0.686274509803922,0.890196078431372);
#13510=COLOUR_RGB('Bearing gray',0.725490196078431,0.752941176470588,0.792156862745098);
#13511=COLOUR_RGB('Axle gray',0.576470588235294,0.615686274509804,0.666666666666667);
#13512=COLOUR_RGB('Dark gray',0.250980392156863,0.282352941176471,0.32156862745098);
#13513=COLOUR_RGB('Bearing light gray',0.725490196078431,0.752941176470588,
0.792156862745098);
ENDSEC;
END-ISO-10303-21;
